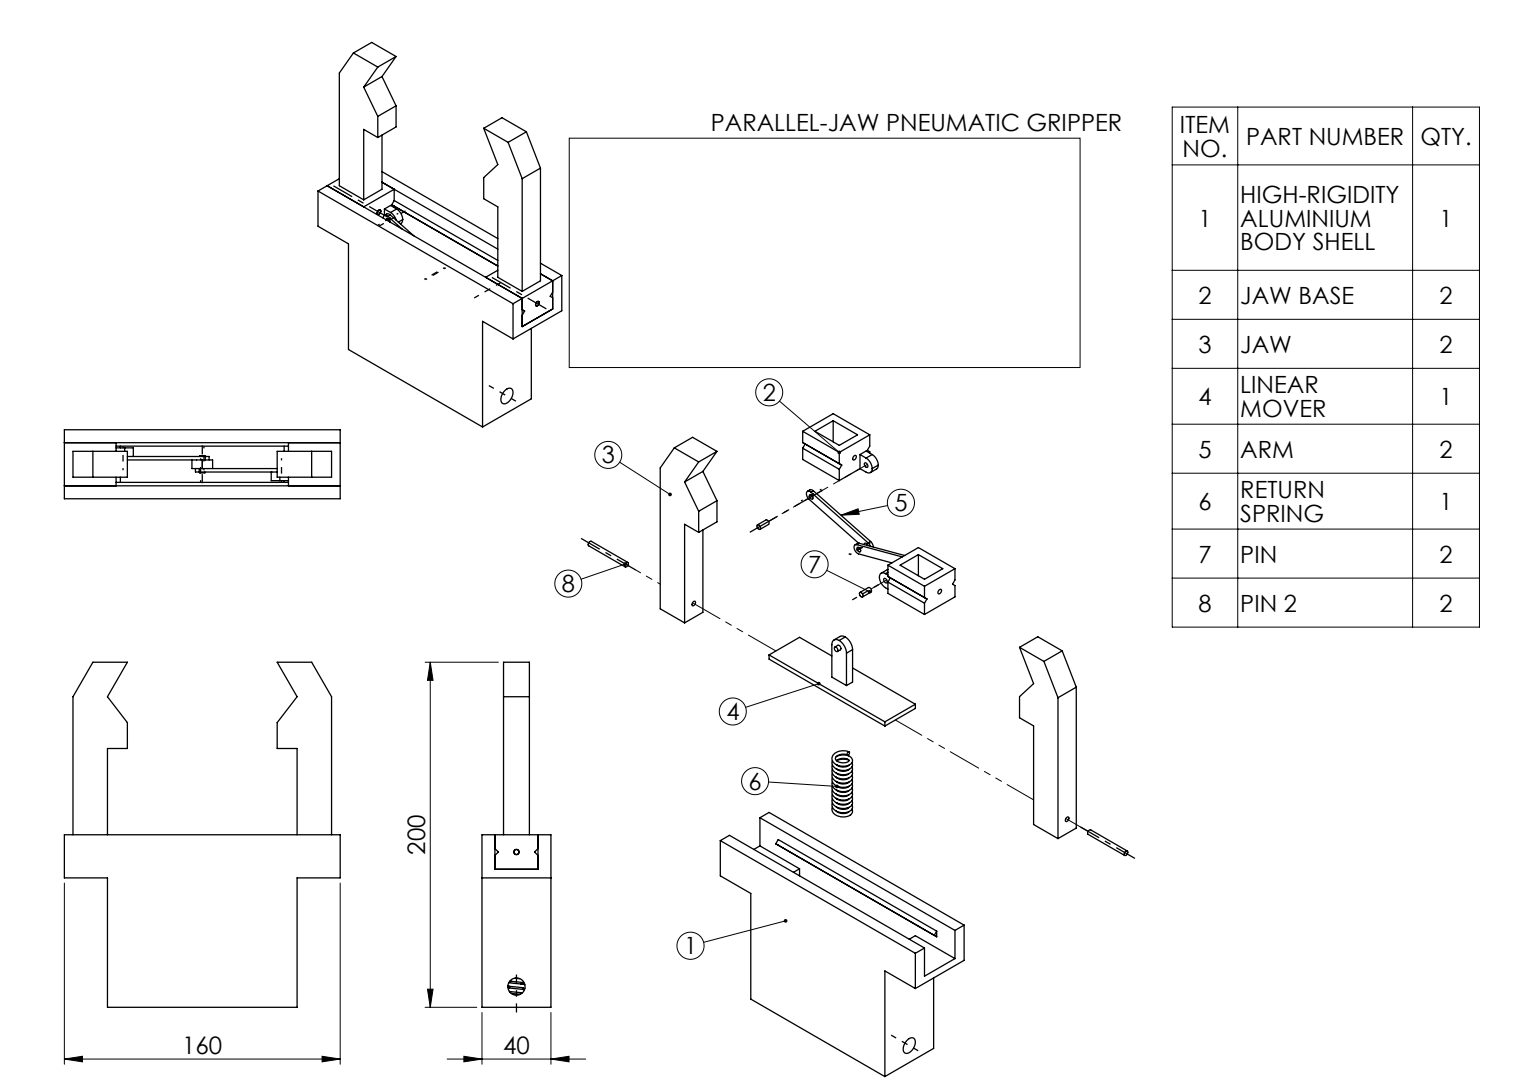
ISO-10303-21;
HEADER;
FILE_DESCRIPTION (('STEP AP214'),
    '1' );
FILE_NAME ('BR-001',
    '2026-10-04T07:56:41',
    ( '' ),
    ( '' ),
    'SwSTEP 2.0',
    'SolidWorks 2026',
    '' );
FILE_SCHEMA (( 'AUTOMOTIVE_DESIGN' ));
ENDSEC;

DATA;
#1 = CARTESIAN_POINT ( 'NONE',  ( 2.179377348189627916, -63.64547149457072805, 7.030887037049939003 ) ) ;
#2 = DIRECTION ( 'NONE',  ( -0.000000000000000000, 2.775557561562891351E-16, -1.000000000000000000 ) ) ;
#3 = CARTESIAN_POINT ( 'NONE',  ( 1.529537955723794918, -69.64547149457074227, 5.030887037049945221 ) ) ;
#4 = CARTESIAN_POINT ( 'NONE',  ( -0.09506052544073731458, -60.49547149457074369, 4.999999999999997335 ) ) ;
#5 = LINE ( 'NONE', #7090, #369 ) ;
#6 = DIRECTION ( 'NONE',  ( -1.000000000000000000, 0.000000000000000000, -0.000000000000000000 ) ) ;
#7 = CARTESIAN_POINT ( 'NONE',  ( -3.015831842038216859, -60.30452850542926058, -3.989209796945429432 ) ) ;
#8 = CARTESIAN_POINT ( 'NONE',  ( -7.360235569667856304, -89.74547149457073658, -0.09995255151716124498 ) ) ;
#9 = VERTEX_POINT ( 'NONE', #7435 ) ;
#10 = CARTESIAN_POINT ( 'NONE',  ( -1.719659006605372076, -75.15452850542925489, -4.969112962950016588 ) ) ;
#11 = DIRECTION ( 'NONE',  ( 0.000000000000000000, -1.000000000000000000, 0.000000000000000000 ) ) ;
#12 = EDGE_CURVE ( 'NONE', #8085, #480, #389, .T. ) ;
#13 = SHAPE_DEFINITION_REPRESENTATION ( #5408, #1019 ) ;
#14 = LINE ( 'NONE', #7738, #5692 ) ;
#15 = CARTESIAN_POINT ( 'NONE',  ( -4.312004677470992142, -84.04547149457074795, 3.009306630940933758 ) ) ;
#16 = CARTESIAN_POINT ( 'NONE',  ( 4.332187097882923332, -97.00000000000000000, -0.04074656551593417581 ) ) ;
#17 = CARTESIAN_POINT ( 'NONE',  ( -2.610703060766926598, -69.04547149457074795, 1.773238653441125745 ) ) ;
#18 = CARTESIAN_POINT ( 'NONE',  ( 6.628020296210641149, -74.40452850542925489, -2.253526892787612645 ) ) ;
#19 = LINE ( 'NONE', #2774, #674 ) ;
#20 = CARTESIAN_POINT ( 'NONE',  ( 4.725907263620373833, -82.09547149457074511, 1.635492904037598283 ) ) ;
#21 = CARTESIAN_POINT ( 'NONE',  ( -5.257311121191324155, -60.75452850542925631, 0.09995255151729526277 ) ) ;
#22 = CARTESIAN_POINT ( 'NONE',  ( -2.862020680886492308, -91.20452850542926626, 4.100960146804039752 ) ) ;
#23 = CARTESIAN_POINT ( 'NONE',  ( -0.09506052544086251999, -66.00452850542926342, -6.999999999999997335 ) ) ;
#24 = CARTESIAN_POINT ( 'NONE',  ( -2.823794231030039015, -86.59547149457075932, -1.017458915287723364 ) ) ;
#25 = VECTOR ( 'NONE', #598, 1000.000000000000000 ) ;
#26 = VERTEX_POINT ( 'NONE', #1027 ) ;
#27 = DIRECTION ( 'NONE',  ( -0.9954714945707483498, -0.09506052544079827971, 1.047588144072330487E-14 ) ) ;
#28 = DIRECTION ( 'NONE',  ( 0.000000000000000000, -1.000000000000000000, 0.000000000000000000 ) ) ;
#29 = CARTESIAN_POINT ( 'NONE',  ( 4.194503406049339134, -89.55452850542926058, -3.171033256558100089 ) ) ;
#30 = EDGE_LOOP ( 'NONE', ( #2065, #6214, #5997, #4915, #7865, #4258, #7605, #3266 ) ) ;
#31 = CARTESIAN_POINT ( 'NONE',  ( 1.529537955723690779, -80.85452850542925773, -5.030887037049978971 ) ) ;
#32 = CARTESIAN_POINT ( 'NONE',  ( 2.493201789345269148, -59.55452850542924637, -1.934965279058294518 ) ) ;
#33 = CARTESIAN_POINT ( 'NONE',  ( 0.000000000000000000, 0.000000000000000000, 0.000000000000000000 ) ) ;
#34 = CARTESIAN_POINT ( 'NONE',  ( -1.719659006605370744, -90.15452850542922647, -4.969112962950016588 ) ) ;
#35 = CARTESIAN_POINT ( 'NONE',  ( 4.037591185471445243, -92.70452850542926626, -5.718994135553947977 ) ) ;
#36 = CARTESIAN_POINT ( 'NONE',  ( -3.015831842038128485, -81.19547149457073942, 3.989209796945492048 ) ) ;
#37 = CARTESIAN_POINT ( 'NONE',  ( 2.823794231030039903, -71.40452850542924068, -1.017458915287783316 ) ) ;
#38 = DIRECTION ( 'NONE',  ( -0.000000000000000000, -0.000000000000000000, -1.000000000000000000 ) ) ;
#39 = CARTESIAN_POINT ( 'NONE',  ( -5.999999999999988454, -100.0010000000000048, -2.499999999999999112 ) ) ;
#40 = CARTESIAN_POINT ( 'NONE',  ( 2.823794231030042123, -89.40452850542926910, -1.017458915287783316 ) ) ;
#41 = CARTESIAN_POINT ( 'NONE',  ( 2.179377348189484476, -95.85452850542924352, -7.030887037049986077 ) ) ;
#42 = VECTOR ( 'NONE', #3900, 1000.000000000000000 ) ;
#43 = EDGE_CURVE ( 'NONE', #1966, #5555, #3595, .T. ) ;
#44 = LINE ( 'NONE', #810, #6447 ) ;
#45 = CARTESIAN_POINT ( 'NONE',  ( 1.719659006605391394, -79.65452850542925489, 4.969112962950016588 ) ) ;
#46 = CARTESIAN_POINT ( 'NONE',  ( 2.369498399071079842, -94.84547149457073090, -6.969112962950057444 ) ) ;
#47 = FACE_OUTER_BOUND ( 'NONE', #854, .T. ) ;
#48 = DIRECTION ( 'NONE',  ( -0.000000000000000000, 1.000000000000000000, 2.775557561562891351E-16 ) ) ;
#49 = VECTOR ( 'NONE', #4022, 1000.000000000000000 ) ;
#50 = AXIS2_PLACEMENT_3D ( 'NONE', #6623, #6543, #5905 ) ;
#51 = CIRCLE ( 'NONE', #1949, 3.000000000000000000 ) ;
#52 = EDGE_CURVE ( 'NONE', #1530, #5461, #2216, .T. ) ;
#53 = CARTESIAN_POINT ( 'NONE',  ( -1.529537955723671905, -61.35452850542925773, 5.030887037049979860 ) ) ;
#54 = CARTESIAN_POINT ( 'NONE',  ( -4.191402346623057440, -87.19547149457073942, 5.607243785695398941 ) ) ;
#55 = VECTOR ( 'NONE', #6929, 1000.000000000000000 ) ;
#56 = ORIENTED_EDGE ( 'NONE', *, *, #5322, .F. ) ;
#57 = CARTESIAN_POINT ( 'NONE',  ( 5.257311121191341918, -71.25452850542923500, -0.09995255151729465215 ) ) ;
#58 = LINE ( 'NONE', #6301, #4909 ) ;
#59 = ITEM_DEFINED_TRANSFORMATION ( 'NONE', 'NONE', #6452,  #2840 ) ;
#60 = CARTESIAN_POINT ( 'NONE',  ( -1.500000000000001110, -27.00000000000000000, 5.000000000000000000 ) ) ;
#61 = CARTESIAN_POINT ( 'NONE',  ( 1.719659006605285922, -76.84547149457073090, -4.969112962950050338 ) ) ;
#62 = CARTESIAN_POINT ( 'NONE',  ( 4.269446988268172483, -97.00000000000001421, -0.4101805542161022777 ) ) ;
#63 = CARTESIAN_POINT ( 'NONE',  ( 0.8796985632579598091, -60.64547149457074227, 3.030887037049952326 ) ) ;
#64 = CARTESIAN_POINT ( 'NONE',  ( 5.895805022753404678, -68.55452850542926058, -4.407101234057908989 ) ) ;
#65 = CARTESIAN_POINT ( 'NONE',  ( -5.999999999999993783, -51.00000000000000711, -2.499999999999999112 ) ) ;
#66 = CARTESIAN_POINT ( 'NONE',  ( -4.194503406049384431, -77.44547149457075363, -3.171033256558012159 ) ) ;
#67 = CARTESIAN_POINT ( 'NONE',  ( 5.257311121191341918, -59.25452850542924210, -0.09995255151729465215 ) ) ;
#68 = CARTESIAN_POINT ( 'NONE',  ( -4.725907263620319654, -87.90452850542926910, 1.635492904037698647 ) ) ;
#69 = CARTESIAN_POINT ( 'NONE',  ( -4.191402346623179120, -72.30452850542926058, -5.607243785695311900 ) ) ;
#70 = EDGE_CURVE ( 'NONE', #8240, #6658, #3048, .T. ) ;
#71 = CARTESIAN_POINT ( 'NONE',  ( -2.823794231030039903, -77.59547149457073090, -1.017458915287723364 ) ) ;
#72 = VERTEX_POINT ( 'NONE', #594 ) ;
#73 = CARTESIAN_POINT ( 'NONE',  ( 3.943604702053941724E-15, -27.99999999999999645, 0.000000000000000000 ) ) ;
#74 = CARTESIAN_POINT ( 'NONE',  ( 54.99999999999999289, 1.301042606982605715E-15, -7.500000000000002665 ) ) ;
#75 = CARTESIAN_POINT ( 'NONE',  ( 2.862020680886515400, -86.70452850542925205, -4.100960146804039752 ) ) ;
#76 = EDGE_LOOP ( 'NONE', ( #356, #276, #5543, #6009 ) ) ;
#77 = CARTESIAN_POINT ( 'NONE',  ( -1.529537955723670128, -79.35452850542925773, 5.030887037049979860 ) ) ;
#78 = CARTESIAN_POINT ( 'NONE',  ( -2.610703060766966566, -63.45452850542924494, -1.773238653441072232 ) ) ;
#79 = DIRECTION ( 'NONE',  ( -1.000000000000000000, 0.000000000000000000, 0.000000000000000000 ) ) ;
#80 = CARTESIAN_POINT ( 'NONE',  ( -2.862020680886493640, -82.20452850542925205, 4.100960146804039752 ) ) ;
#81 = CARTESIAN_POINT ( 'NONE',  ( 2.369498399071075845, -64.84547149457071669, -6.969112962950057444 ) ) ;
#82 = CARTESIAN_POINT ( 'NONE',  ( 1.069819614139556396, -70.65452850542925489, 2.969112962950023249 ) ) ;
#83 = EDGE_CURVE ( 'NONE', #4707, #1590, #2672, .T. ) ;
#84 = DIRECTION ( 'NONE',  ( 0.000000000000000000, -1.000000000000000000, -1.734723475976807094E-16 ) ) ;
#85 = DIRECTION ( 'NONE',  ( 0.000000000000000000, 0.000000000000000000, 1.000000000000000000 ) ) ;
#86 = CARTESIAN_POINT ( 'NONE',  ( 3.154386672714810658, -89.25452850542926342, -0.09995255151727241993 ) ) ;
#87 = CARTESIAN_POINT ( 'NONE',  ( 4.191402346623199549, -94.80452850542926058, 5.607243785695311900 ) ) ;
#88 = FACE_OUTER_BOUND ( 'NONE', #2763, .T. ) ;
#89 = CARTESIAN_POINT ( 'NONE',  ( 1.529537955723689890, -74.85452850542925773, -5.030887037049978971 ) ) ;
#90 = CARTESIAN_POINT ( 'NONE',  ( -5.895805022753476621, -89.44547149457073942, -4.407101234057782868 ) ) ;
#91 = DIRECTION ( 'NONE',  ( 1.000000000000000000, -0.000000000000000000, -0.000000000000000000 ) ) ;
#92 = CARTESIAN_POINT ( 'NONE',  ( -47.50000000000000711, 47.23441352194253540, 12.50000000000001954 ) ) ;
#93 = CARTESIAN_POINT ( 'NONE',  ( -0.09506052544075821453, -63.49547149457075079, 2.999999999999997780 ) ) ;
#94 = ADVANCED_FACE ( 'NONE', ( #2381 ), #5021, .T. ) ;
#95 = CARTESIAN_POINT ( 'NONE',  ( -4.312004677471060532, -60.45452850542923784, -3.009306630940844052 ) ) ;
#96 = CARTESIAN_POINT ( 'NONE',  ( -6.013306294175058575, -87.04547149457074795, 4.245374608440741326 ) ) ;
#97 = VERTEX_POINT ( 'NONE', #4421 ) ;
#98 = AXIS2_PLACEMENT_3D ( 'NONE', #2797, #1653, #1018 ) ;
#99 = CARTESIAN_POINT ( 'NONE',  ( -3.015831842038215083, -75.30452850542926058, -3.989209796945429432 ) ) ;
#100 = CARTESIAN_POINT ( 'NONE',  ( 50.00000000000000000, -1.734723475976807094E-15, 12.50000000000000000 ) ) ;
#101 = CARTESIAN_POINT ( 'NONE',  ( 46.73922289128223895, -17.64104216824340199, 4.500000000000000888 ) ) ;
#102 = EDGE_CURVE ( 'NONE', #5844, #6402, #2825, .T. ) ;
#103 = CARTESIAN_POINT ( 'NONE',  ( 2.862020680886599333, -78.79547149457074795, 4.100960146803977580 ) ) ;
#104 = DIRECTION ( 'NONE',  ( 0.000000000000000000, -1.000000000000000000, 0.000000000000000000 ) ) ;
#105 = CARTESIAN_POINT ( 'NONE',  ( -1.840261337453202639, -60.19547149457074653, 2.371175808195584267 ) ) ;
#106 = CARTESIAN_POINT ( 'NONE',  ( 6.686770931921523164, -65.10452850542924352, 2.072711028461649008 ) ) ;
#107 = LINE ( 'NONE', #2692, #5969 ) ;
#108 = CARTESIAN_POINT ( 'NONE',  ( 1.529537955723795584, -81.64547149457074227, 5.030887037049945221 ) ) ;
#109 = DIRECTION ( 'NONE',  ( -0.000000000000000000, 0.000000000000000000, -1.000000000000000000 ) ) ;
#110 = CARTESIAN_POINT ( 'NONE',  ( 3.015831842038235511, -88.80452850542926058, 3.989209796945429432 ) ) ;
#111 = CARTESIAN_POINT ( 'NONE',  ( -6.013306294175152722, -72.45452850542925205, -4.245374608440613429 ) ) ;
#112 = CARTESIAN_POINT ( 'NONE',  ( 3.154386672714809770, -79.24547149457073658, 0.09995255151720662534 ) ) ;
#113 = EDGE_CURVE ( 'NONE', #4681, #4928, #8269, .T. ) ;
#114 = ORIENTED_EDGE ( 'NONE', *, *, #1617, .T. ) ;
#115 = AXIS2_PLACEMENT_3D ( 'NONE', #3789, #4326, #6319 ) ;
#116 = DIRECTION ( 'NONE',  ( 0.000000000000000000, 0.000000000000000000, 1.000000000000000000 ) ) ;
#117 = CARTESIAN_POINT ( 'NONE',  ( 47.50000000000002132, 47.23441352194253540, 12.50000000000001954 ) ) ;
#118 = CARTESIAN_POINT ( 'NONE',  ( -2.862020680886492308, -91.20452850542926626, 4.100960146804039752 ) ) ;
#119 = ORIENTED_EDGE ( 'NONE', *, *, #70, .T. ) ;
#120 = CARTESIAN_POINT ( 'NONE',  ( 4.725907263620340970, -80.40452850542925489, -1.635492904037697981 ) ) ;
#121 = CARTESIAN_POINT ( 'NONE',  ( 2.610703060766946582, -88.54547149457074795, -1.773238653441125523 ) ) ;
#122 = DIRECTION ( 'NONE',  ( 1.000000000000000000, 0.000000000000000000, 0.000000000000000000 ) ) ;
#123 = CARTESIAN_POINT ( 'NONE',  ( -0.09506052544083921918, -84.00452850542926342, -4.999999999999997335 ) ) ;
#124 = AXIS2_PLACEMENT_3D ( 'NONE', #3381, #3919, #122 ) ;
#125 = CARTESIAN_POINT ( 'NONE',  ( 0.09506052544073236021, -61.99547149457073658, -6.999999999999997335 ) ) ;
#126 = VECTOR ( 'NONE', #38, 1000.000000000000000 ) ;
#127 = CARTESIAN_POINT ( 'NONE',  ( -1.840261337453252821, -69.30452850542926058, -2.371175808195547852 ) ) ;
#128 = FACE_OUTER_BOUND ( 'NONE', #7423, .T. ) ;
#129 = AXIS2_PLACEMENT_3D ( 'NONE', #1955, #4587, #1439 ) ;
#130 = DIRECTION ( 'NONE',  ( -1.000000000000000000, 0.000000000000000000, 0.000000000000000000 ) ) ;
#131 = CARTESIAN_POINT ( 'NONE',  ( 1.069819614139557284, -79.65452850542925489, 2.969112962950023249 ) ) ;
#132 = CARTESIAN_POINT ( 'NONE',  ( 7.360235569667880284, -92.25452850542926342, -0.09995255151731691212 ) ) ;
#133 = FACE_OUTER_BOUND ( 'NONE', #6862, .T. ) ;
#134 = CARTESIAN_POINT ( 'NONE',  ( -6.628020296210666018, -86.59547149457075932, -2.253526892787471869 ) ) ;
#135 = CARTESIAN_POINT ( 'NONE',  ( -65.00000000000000000, -7.999999999999992895, -12.50000000000000178 ) ) ;
#136 = CARTESIAN_POINT ( 'NONE',  ( -65.00000000000000000, -12.00000000000000711, 12.49999999999999822 ) ) ;
#137 = PRESENTATION_LAYER_ASSIGNMENT (  '', '', ( #6998 ) ) ;
#138 = CARTESIAN_POINT ( 'NONE',  ( -0.8796985632579439329, -68.14547149457074227, -3.030887037049952326 ) ) ;
#139 = CARTESIAN_POINT ( 'NONE',  ( -4.194503406049321370, -58.05452850542925347, 3.171033256558100533 ) ) ;
#140 = VERTEX_POINT ( 'NONE', #4384 ) ;
#141 = CARTESIAN_POINT ( 'NONE',  ( 4.312004677471075631, -73.95452850542926626, 3.009306630940844496 ) ) ;
#142 = CARTESIAN_POINT ( 'NONE',  ( -0.09506052544071266763, -87.49547149457075079, 6.999999999999997335 ) ) ;
#143 = ORIENTED_EDGE ( 'NONE', *, *, #1238, .T. ) ;
#144 = CARTESIAN_POINT ( 'NONE',  ( 0.09506052544086046607, -79.50452850542926342, 4.999999999999997335 ) ) ;
#145 = CARTESIAN_POINT ( 'NONE',  ( -80.00000000000000000, -50.00000000000000711, -12.50000000000000888 ) ) ;
#146 = CARTESIAN_POINT ( 'NONE',  ( 55.00000000000002132, -93.00000000000000000, 6.123233995736772199E-16 ) ) ;
#147 = CARTESIAN_POINT ( 'NONE',  ( -4.312004677470993030, -78.04547149457076216, 3.009306630940933758 ) ) ;
#148 = LINE ( 'NONE', #5288, #6329 ) ;
#149 = CARTESIAN_POINT ( 'NONE',  ( -2.610703060766927930, -63.04547149457074084, 1.773238653441125745 ) ) ;
#150 = CARTESIAN_POINT ( 'NONE',  ( -5.895805022753386915, -67.05452850542926058, 4.407101234057909878 ) ) ;
#151 = LINE ( 'NONE', #65, #1132 ) ;
#152 = CARTESIAN_POINT ( 'NONE',  ( -5.257311121191324155, -74.74547149457075079, -0.09995255151718371311 ) ) ;
#153 = SHAPE_REPRESENTATION ( 'pin 2', ( #2840 ), #1883 ) ;
#154 = LINE ( 'NONE', #7878, #4231 ) ;
#155 = CARTESIAN_POINT ( 'NONE',  ( 0.09506052544086084077, -82.50452850542926342, 4.999999999999997335 ) ) ;
#156 = CARTESIAN_POINT ( 'NONE',  ( 6.686770931921523164, -68.10452850542924352, 2.072711028461649008 ) ) ;
#157 = CARTESIAN_POINT ( 'NONE',  ( 0.8796985632579618075, -75.64547149457072805, 3.030887037049952326 ) ) ;
#158 = EDGE_CURVE ( 'NONE', #4876, #5889, #5061, .T. ) ;
#159 = EDGE_LOOP ( 'NONE', ( #4079, #1702, #1986 ) ) ;
#160 = FACE_OUTER_BOUND ( 'NONE', #6946, .T. ) ;
#161 = CARTESIAN_POINT ( 'NONE',  ( 2.862020680886516732, -95.70452850542926626, -4.100960146804039752 ) ) ;
#162 = CARTESIAN_POINT ( 'NONE',  ( 3.015831842038235511, -88.80452850542926058, 3.989209796945429432 ) ) ;
#163 = EDGE_LOOP ( 'NONE', ( #6818, #3032, #7905, #4249 ) ) ;
#164 = CARTESIAN_POINT ( 'NONE',  ( -2.862020680886494084, -79.20452850542925205, 4.100960146804039752 ) ) ;
#165 = CARTESIAN_POINT ( 'NONE',  ( -3.154386672714787565, -89.74547149457073658, -0.09995255151720625064 ) ) ;
#166 = CARTESIAN_POINT ( 'NONE',  ( 1.719659006605392504, -88.65452850542925489, 4.969112962950016588 ) ) ;
#167 = EDGE_CURVE ( 'NONE', #2862, #1798, #3763, .T. ) ;
#168 = CARTESIAN_POINT ( 'NONE',  ( -6.013306294175062128, -60.04547149457073374, 4.245374608440741326 ) ) ;
#169 = CARTESIAN_POINT ( 'NONE',  ( -1.686450176301567350, -64.20452850542925205, 2.482926158054133303 ) ) ;
#170 = CARTESIAN_POINT ( 'NONE',  ( 80.00000000000000000, 0.000000000000000000, 20.00000000000000000 ) ) ;
#171 = FACE_OUTER_BOUND ( 'NONE', #565, .T. ) ;
#172 = CARTESIAN_POINT ( 'NONE',  ( 0.8796985632578988579, -74.85452850542925773, -3.030887037049972310 ) ) ;
#173 = CARTESIAN_POINT ( 'NONE',  ( -2.179377348189460051, -88.35452850542924352, 7.030887037049988741 ) ) ;
#174 = CARTESIAN_POINT ( 'NONE',  ( 1.500000000000002442, -27.00000000000000000, 5.000000000000000000 ) ) ;
#175 = CARTESIAN_POINT ( 'NONE',  ( -4.037591185471542943, -89.29547149457074795, -5.718994135553860936 ) ) ;
#176 = CYLINDRICAL_SURFACE ( 'NONE', #6965, 5.000000000000004441 ) ;
#177 = LINE ( 'NONE', #1487, #3670 ) ;
#178 = CARTESIAN_POINT ( 'NONE',  ( -1.069819614139475794, -66.34547149457073090, 2.969112962950044121 ) ) ;
#179 = CARTESIAN_POINT ( 'NONE',  ( -4.725907263620323207, -63.90452850542925489, 1.635492904037698647 ) ) ;
#180 = VECTOR ( 'NONE', #3060, 1000.000000000000000 ) ;
#181 = ORIENTED_EDGE ( 'NONE', *, *, #5142, .F. ) ;
#182 = CARTESIAN_POINT ( 'NONE',  ( 5.257311121191341918, -71.25452850542923500, -0.09995255151729465215 ) ) ;
#183 = CARTESIAN_POINT ( 'NONE',  ( 0.09506052544073499699, -82.99547149457075079, -6.999999999999997335 ) ) ;
#184 = VERTEX_POINT ( 'NONE', #4941 ) ;
#185 = CARTESIAN_POINT ( 'NONE',  ( 1.529537955723690112, -77.85452850542922931, -5.030887037049978971 ) ) ;
#186 = EDGE_CURVE ( 'NONE', #2522, #3855, #7004, .T. ) ;
#187 = VECTOR ( 'NONE', #1383, 1000.000000000000000 ) ;
#188 = PLANE ( 'NONE',  #457 ) ;
#189 = AXIS2_PLACEMENT_3D ( 'NONE', #3637, #5920, #5243 ) ;
#190 = VECTOR ( 'NONE', #1369, 1000.000000000000000 ) ;
#191 = CARTESIAN_POINT ( 'NONE',  ( 3.015831842038148025, -70.69547149457073942, -3.989209796945492048 ) ) ;
#192 = FACE_OUTER_BOUND ( 'NONE', #662, .T. ) ;
#193 = CARTESIAN_POINT ( 'NONE',  ( -1.686450176301618642, -65.29547149457073374, -2.482926158054096000 ) ) ;
#194 = CARTESIAN_POINT ( 'NONE',  ( 7.360235569667877620, -74.25452850542924921, -0.09995255151731691212 ) ) ;
#195 = CARTESIAN_POINT ( 'NONE',  ( 80.00000000000000000, 0.000000000000000000, 20.00000000000000000 ) ) ;
#196 = FILL_AREA_STYLE_COLOUR ( '', #1408 ) ;
#197 = CARTESIAN_POINT ( 'NONE',  ( 1.529537955723691001, -83.85452850542927195, -5.030887037049978971 ) ) ;
#198 = CARTESIAN_POINT ( 'NONE',  ( -6.628020296210623385, -63.90452850542925489, 2.253526892787613978 ) ) ;
#199 = CARTESIAN_POINT ( 'NONE',  ( -1.069819614139474906, -75.34547149457073090, 2.969112962950044121 ) ) ;
#200 = VERTEX_POINT ( 'NONE', #6335 ) ;
#201 = CARTESIAN_POINT ( 'NONE',  ( 80.00000000000000000, 0.000000000000000000, 20.00000000000000000 ) ) ;
#202 = CARTESIAN_POINT ( 'NONE',  ( -1.719659006605370744, -93.15452850542925489, -4.969112962950016588 ) ) ;
#203 = CARTESIAN_POINT ( 'NONE',  ( 4.725907263620340970, -83.40452850542925489, -1.635492904037697981 ) ) ;
#204 = VERTEX_POINT ( 'NONE', #1706 ) ;
#205 = CARTESIAN_POINT ( 'NONE',  ( 5.257311121191341030, -71.25452850542924921, -0.09995255151729466603 ) ) ;
#206 = CARTESIAN_POINT ( 'NONE',  ( 2.610703060766947914, -94.54547149457073374, -1.773238653441125523 ) ) ;
#207 = CARTESIAN_POINT ( 'NONE',  ( -4.194503406049315153, -91.05452850542923215, 3.171033256558100533 ) ) ;
#208 = CARTESIAN_POINT ( 'NONE',  ( 6.013306294175077227, -61.54547149457074084, -4.245374608440741326 ) ) ;
#209 = CARTESIAN_POINT ( 'NONE',  ( -1.840261337453252821, -66.30452850542926058, -2.371175808195547852 ) ) ;
#210 = VERTEX_POINT ( 'NONE', #510 ) ;
#211 = DIRECTION ( 'NONE',  ( 9.251858538542971581E-17, -1.000000000000000000, 0.000000000000000000 ) ) ;
#212 = CARTESIAN_POINT ( 'NONE',  ( -0.9662349396012467340, -27.25766265056033433, 4.500000000000000888 ) ) ;
#213 = CARTESIAN_POINT ( 'NONE',  ( -1.686450176301564907, -82.20452850542925205, 2.482926158054133303 ) ) ;
#214 = CARTESIAN_POINT ( 'NONE',  ( 2.179377348189483143, -86.85452850542924352, -7.030887037049986077 ) ) ;
#215 = CARTESIAN_POINT ( 'NONE',  ( -4.191402346623057440, -87.19547149457073942, 5.607243785695398941 ) ) ;
#216 = CARTESIAN_POINT ( 'NONE',  ( -5.999999999999992895, -50.00000000000000000, -2.499999999999999112 ) ) ;
#217 = DIRECTION ( 'NONE',  ( 0.000000000000000000, 0.7071067811865507924, -0.7071067811865441310 ) ) ;
#218 = CARTESIAN_POINT ( 'NONE',  ( -0.09506052544075743738, -69.49547149457075079, 2.999999999999997780 ) ) ;
#219 = UNCERTAINTY_MEASURE_WITH_UNIT (LENGTH_MEASURE( 1.000000000000000082E-05 ), #2470, 'distance_accuracy_value', 'NONE');
#220 = SURFACE_SIDE_STYLE ('',( #2333 ) ) ;
#221 = ORIENTED_EDGE ( 'NONE', *, *, #2206, .T. ) ;
#222 = ADVANCED_FACE ( 'NONE', ( #7515 ), #5686, .T. ) ;
#223 = CARTESIAN_POINT ( 'NONE',  ( -4.194503406049319594, -67.05452850542926058, 3.171033256558100533 ) ) ;
#224 = CARTESIAN_POINT ( 'NONE',  ( 6.628020296210687334, -79.09547149457075932, 2.253526892787472757 ) ) ;
#225 = SURFACE_STYLE_FILL_AREA ( #2174 ) ;
#226 = EDGE_CURVE ( 'NONE', #6118, #4574, #2581, .T. ) ;
#227 = ORIENTED_EDGE ( 'NONE', *, *, #6640, .F. ) ;
#228 = CARTESIAN_POINT ( 'NONE',  ( -5.257311121191324155, -63.75452850542925631, 0.09995255151729526277 ) ) ;
#229 = CARTESIAN_POINT ( 'NONE',  ( -5.999999999999993783, -51.00000000000000711, 2.500000000000000888 ) ) ;
#230 = CARTESIAN_POINT ( 'NONE',  ( -5.257311121191324155, -71.74547149457075079, -0.09995255151718371311 ) ) ;
#231 = CARTESIAN_POINT ( 'NONE',  ( -80.00100000000001899, -83.00000000000002842, 0.000000000000000000 ) ) ;
#232 = CARTESIAN_POINT ( 'NONE',  ( 1.719659006605287921, -97.84547149457071669, -4.969112962950050338 ) ) ;
#233 = CARTESIAN_POINT ( 'NONE',  ( 6.686770931921522276, -62.10452850542925063, 2.072711028461649008 ) ) ;
#234 = ORIENTED_EDGE ( 'NONE', *, *, #7378, .T. ) ;
#235 = CARTESIAN_POINT ( 'NONE',  ( 1.719659006605391616, -82.65452850542925489, 4.969112962950016588 ) ) ;
#236 = CARTESIAN_POINT ( 'NONE',  ( 6.628020296210639373, -62.40452850542925489, -2.253526892787612645 ) ) ;
#237 = CARTESIAN_POINT ( 'NONE',  ( 2.882544866740877065, -73.39547149457074227, -0.8366430509619593447 ) ) ;
#238 = VERTEX_POINT ( 'NONE', #7087 ) ;
#239 = DIRECTION ( 'NONE',  ( 0.000000000000000000, -0.000000000000000000, -1.000000000000000000 ) ) ;
#240 = CARTESIAN_POINT ( 'NONE',  ( 3.015831842038236399, -94.80452850542924637, 3.989209796945429432 ) ) ;
#241 = CARTESIAN_POINT ( 'NONE',  ( 1.529537955723690112, -77.85452850542922931, -5.030887037049978971 ) ) ;
#242 = ORIENTED_EDGE ( 'NONE', *, *, #358, .F. ) ;
#243 = CARTESIAN_POINT ( 'NONE',  ( -4.312004677471057867, -72.45452850542923784, -3.009306630940843608 ) ) ;
#244 = CARTESIAN_POINT ( 'NONE',  ( -0.8796985632579418235, -86.14547149457072805, -3.030887037049952326 ) ) ;
#245 = CARTESIAN_POINT ( 'NONE',  ( 2.862020680886601998, -96.79547149457073374, 4.100960146803977580 ) ) ;
#246 = CARTESIAN_POINT ( 'NONE',  ( 0.09506052544086046607, -79.50452850542926342, 4.999999999999997335 ) ) ;
#247 = CARTESIAN_POINT ( 'NONE',  ( 2.369498399071225947, -85.65452850542926910, 6.969112962950009482 ) ) ;
#248 = ADVANCED_FACE ( 'NONE', ( #3343 ), #5902, .T. ) ;
#249 = CARTESIAN_POINT ( 'NONE',  ( 1.686450176301584225, -68.70452850542925205, -2.482926158054133303 ) ) ;
#250 = VERTEX_POINT ( 'NONE', #3258 ) ;
#251 = FACE_OUTER_BOUND ( 'NONE', #7883, .T. ) ;
#252 = LINE ( 'NONE', #8058, #5108 ) ;
#253 = CARTESIAN_POINT ( 'NONE',  ( 1.686450176301585335, -77.70452850542925205, -2.482926158054133303 ) ) ;
#254 = CARTESIAN_POINT ( 'NONE',  ( 7.360235569667880284, -86.25452850542924921, -0.09995255151731691212 ) ) ;
#255 = AXIS2_PLACEMENT_3D ( 'NONE', #6696, #2244, #926 ) ;
#256 = CARTESIAN_POINT ( 'NONE',  ( 4.191402346623080533, -88.69547149457073942, -5.607243785695398941 ) ) ;
#257 = DIRECTION ( 'NONE',  ( 0.000000000000000000, 0.000000000000000000, 1.000000000000000000 ) ) ;
#258 = PRODUCT_RELATED_PRODUCT_CATEGORY ( 'part', '', ( #6217 ) ) ;
#259 = DIRECTION ( 'NONE',  ( 0.000000000000000000, 0.7071067811865442421, -0.7071067811865509034 ) ) ;
#260 = CARTESIAN_POINT ( 'NONE',  ( 0.09506052544077478461, -64.99547149457075079, -2.999999999999997780 ) ) ;
#261 = CARTESIAN_POINT ( 'NONE',  ( 46.73922289128223895, -17.64104216824340199, 4.500000000000000888 ) ) ;
#262 = ORIENTED_EDGE ( 'NONE', *, *, #5429, .F. ) ;
#263 = CARTESIAN_POINT ( 'NONE',  ( 3.015831842038232402, -64.80452850542926058, 3.989209796945429432 ) ) ;
#264 = CARTESIAN_POINT ( 'NONE',  ( 2.369498399071077177, -76.84547149457073090, -6.969112962950057444 ) ) ;
#265 = FILL_AREA_STYLE ('',( #2132 ) ) ;
#266 = CARTESIAN_POINT ( 'NONE',  ( 54.99999999999999289, -1.301042606982604729E-15, 7.499999999999997335 ) ) ;
#267 = VECTOR ( 'NONE', #2809, 1000.000000000000000 ) ;
#268 = CARTESIAN_POINT ( 'NONE',  ( -1.719659006605265716, -75.34547149457074511, 4.969112962950051227 ) ) ;
#269 = CARTESIAN_POINT ( 'NONE',  ( -0.09506052544084110656, -69.00452850542926342, -4.999999999999997335 ) ) ;
#270 = DIRECTION ( 'NONE',  ( -0.000000000000000000, -0.000000000000000000, -1.000000000000000000 ) ) ;
#271 = CIRCLE ( 'NONE', #522, 5.000000000000000888 ) ;
#272 = CARTESIAN_POINT ( 'NONE',  ( -4.784657899331159925, -65.89547149457074227, 1.454677039711874675 ) ) ;
#273 = DIRECTION ( 'NONE',  ( 0.000000000000000000, 0.000000000000000000, 1.000000000000000000 ) ) ;
#274 = CARTESIAN_POINT ( 'NONE',  ( -4.784657899331155484, -95.89547149457074227, 1.454677039711874675 ) ) ;
#275 = CARTESIAN_POINT ( 'NONE',  ( -6.013306294175153610, -60.45452850542925916, -4.245374608440613429 ) ) ;
#276 = ORIENTED_EDGE ( 'NONE', *, *, #1868, .F. ) ;
#277 = ADVANCED_FACE ( 'NONE', ( #133 ), #3970, .F. ) ;
#278 = FILL_AREA_STYLE ('',( #196 ) ) ;
#279 = CARTESIAN_POINT ( 'NONE',  ( 1.529537955723690557, -80.85452850542925773, -5.030887037049978971 ) ) ;
#280 = EDGE_CURVE ( 'NONE', #6915, #2088, #1958, .T. ) ;
#281 = ORIENTED_EDGE ( 'NONE', *, *, #3692, .F. ) ;
#282 = DIRECTION ( 'NONE',  ( 0.000000000000000000, -2.775557561562891351E-16, 1.000000000000000000 ) ) ;
#283 = CARTESIAN_POINT ( 'NONE',  ( -4.312004677471056091, -87.45452850542925205, -3.009306630940844052 ) ) ;
#284 = CARTESIAN_POINT ( 'NONE',  ( -1.529537955723669684, -82.35452850542922931, 5.030887037049979860 ) ) ;
#285 = ORIENTED_EDGE ( 'NONE', *, *, #8144, .T. ) ;
#286 = CARTESIAN_POINT ( 'NONE',  ( -0.09506052544084110656, -69.00452850542926342, -4.999999999999997335 ) ) ;
#287 = CARTESIAN_POINT ( 'NONE',  ( 2.493201789345311337, -87.94547149457073942, 1.934965279058241006 ) ) ;
#288 = CARTESIAN_POINT ( 'NONE',  ( -2.493201789345293129, -59.44547149457074653, -1.934965279058240561 ) ) ;
#289 = CARTESIAN_POINT ( 'NONE',  ( 1.719659006605391172, -76.65452850542922647, 4.969112962950016588 ) ) ;
#290 = CARTESIAN_POINT ( 'NONE',  ( 6.628020296210642037, -86.40452850542926910, -2.253526892787612645 ) ) ;
#291 = ADVANCED_FACE ( 'NONE', ( #7854, #719 ), #1914, .F. ) ;
#292 = CARTESIAN_POINT ( 'NONE',  ( -2.493201789345288688, -95.44547149457075363, -1.934965279058240561 ) ) ;
#293 = VERTEX_POINT ( 'NONE', #7045 ) ;
#294 = CARTESIAN_POINT ( 'NONE',  ( 6.123233995736760366E-16, -27.00000000000000000, -5.000000000000000000 ) ) ;
#295 = CARTESIAN_POINT ( 'NONE',  ( 54.99999999999999289, 1.301042606982605715E-15, -7.500000000000002665 ) ) ;
#296 = CARTESIAN_POINT ( 'NONE',  ( 1.840261337453271473, -82.80452850542926058, 2.371175808195547852 ) ) ;
#297 = CARTESIAN_POINT ( 'NONE',  ( -7.360235569667856304, -87.75452850542924921, 0.09995255151731782806 ) ) ;
#298 = CARTESIAN_POINT ( 'NONE',  ( 2.369498399071078065, -79.84547149457074511, -6.969112962950057444 ) ) ;
#299 = CARTESIAN_POINT ( 'NONE',  ( 50.00000000000000000, 1.734723475976807094E-15, -12.50000000000000000 ) ) ;
#300 = CARTESIAN_POINT ( 'NONE',  ( 2.862020680886601554, -93.79547149457074795, 4.100960146803977580 ) ) ;
#301 = CARTESIAN_POINT ( 'NONE',  ( -0.8796985632578785408, -82.35452850542927195, 3.030887037049973198 ) ) ;
#302 = UNCERTAINTY_MEASURE_WITH_UNIT (LENGTH_MEASURE( 1.000000000000000082E-05 ), #4684, 'distance_accuracy_value', 'NONE');
#303 = FACE_OUTER_BOUND ( 'NONE', #1052, .T. ) ;
#304 = ORIENTED_EDGE ( 'NONE', *, *, #4864, .F. ) ;
#305 = CARTESIAN_POINT ( 'NONE',  ( 54.99999999999999289, -9.999999999999994671, -1.500000000000000666 ) ) ;
#306 = CARTESIAN_POINT ( 'NONE',  ( -5.257311121191324155, -63.75452850542925631, 0.09995255151729526277 ) ) ;
#307 = CARTESIAN_POINT ( 'NONE',  ( -2.369498399071056305, -84.34547149457075932, 6.969112962950058332 ) ) ;
#308 = ORIENTED_EDGE ( 'NONE', *, *, #7858, .F. ) ;
#309 = CARTESIAN_POINT ( 'NONE',  ( 1.529537955723795584, -75.64547149457072805, 5.030887037049945221 ) ) ;
#310 = CARTESIAN_POINT ( 'NONE',  ( 4.784657899331176800, -73.39547149457074227, -1.454677039711874009 ) ) ;
#311 = CARTESIAN_POINT ( 'NONE',  ( -4.194503406049319594, -67.05452850542926058, 3.171033256558100533 ) ) ;
#312 = CARTESIAN_POINT ( 'NONE',  ( -5.999999999999988454, -100.0010000000000048, 2.500000000000000888 ) ) ;
#313 = CARTESIAN_POINT ( 'NONE',  ( 1.529537955723795140, -69.64547149457074227, 5.030887037049945221 ) ) ;
#314 = CARTESIAN_POINT ( 'NONE',  ( 45.00000000000000000, -14.99999999999999467, 4.499999999999999112 ) ) ;
#315 = CARTESIAN_POINT ( 'NONE',  ( -6.686770931921508954, -57.60452850542926484, -2.072711028461647675 ) ) ;
#316 = ORIENTED_EDGE ( 'NONE', *, *, #6930, .F. ) ;
#317 = AXIS2_PLACEMENT_3D ( 'NONE', #4788, #4662, #4742 ) ;
#318 = LINE ( 'NONE', #2975, #6253 ) ;
#319 = AXIS2_PLACEMENT_3D ( 'NONE', #8320, #7056, #3853 ) ;
#320 = ORIENTED_EDGE ( 'NONE', *, *, #4393, .F. ) ;
#321 = CARTESIAN_POINT ( 'NONE',  ( 55.00000000000000000, -25.00000000000002132, 20.00000000000000000 ) ) ;
#322 = CARTESIAN_POINT ( 'NONE',  ( -4.194503406049315153, -88.05452850542921794, 3.171033256558100533 ) ) ;
#323 = CARTESIAN_POINT ( 'NONE',  ( -4.312004677471057867, -78.45452850542925205, -3.009306630940844052 ) ) ;
#324 = ORIENTED_EDGE ( 'NONE', *, *, #6025, .F. ) ;
#325 = CARTESIAN_POINT ( 'NONE',  ( 1.719659006605389839, -67.65452850542925489, 4.969112962950015699 ) ) ;
#326 = CARTESIAN_POINT ( 'NONE',  ( 0.09506052544077665811, -79.99547149457075079, -2.999999999999997780 ) ) ;
#327 = CARTESIAN_POINT ( 'NONE',  ( -4.312004677470990366, -96.04547149457074795, 3.009306630940933758 ) ) ;
#328 = EDGE_CURVE ( 'NONE', #3916, #5740, #1998, .T. ) ;
#329 = CARTESIAN_POINT ( 'NONE',  ( -4.194503406049316929, -73.05452850542926058, 3.171033256558100533 ) ) ;
#330 = CARTESIAN_POINT ( 'NONE',  ( -6.013306294175149169, -87.45452850542925205, -4.245374608440613429 ) ) ;
#331 = CARTESIAN_POINT ( 'NONE',  ( 2.823794231030038571, -59.40452850542925489, -1.017458915287783316 ) ) ;
#332 = ORIENTED_EDGE ( 'NONE', *, *, #7144, .F. ) ;
#333 = PLANE ( 'NONE',  #3355 ) ;
#334 = ORIENTED_EDGE ( 'NONE', *, *, #1098, .F. ) ;
#335 = DIRECTION ( 'NONE',  ( 0.000000000000000000, -1.000000000000000000, 0.000000000000000000 ) ) ;
#336 = CARTESIAN_POINT ( 'NONE',  ( 2.823794231030039903, -71.40452850542924068, -1.017458915287783316 ) ) ;
#337 = CARTESIAN_POINT ( 'NONE',  ( -6.013306294175152722, -78.45452850542925205, -4.245374608440613429 ) ) ;
#338 = CARTESIAN_POINT ( 'NONE',  ( -6.628020296210667794, -80.59547149457075932, -2.253526892787471869 ) ) ;
#339 = CARTESIAN_POINT ( 'NONE',  ( 6.000000000000012434, -50.00000000000000000, 2.500000000000000888 ) ) ;
#340 = CARTESIAN_POINT ( 'NONE',  ( -4.784657899331155484, -95.89547149457074227, 1.454677039711874675 ) ) ;
#341 = CARTESIAN_POINT ( 'NONE',  ( 0.8796985632579006342, -89.85452850542924352, -3.030887037049972310 ) ) ;
#342 = SURFACE_STYLE_USAGE ( .BOTH. , #220 ) ;
#343 = ORIENTED_EDGE ( 'NONE', *, *, #113, .F. ) ;
#344 = CARTESIAN_POINT ( 'NONE',  ( 80.00000000000000000, -9.999999999999991118, -10.50000000000000888 ) ) ;
#345 = CARTESIAN_POINT ( 'NONE',  ( -2.882544866740875289, -93.60452850542925773, -0.8366430509618996147 ) ) ;
#346 = CARTESIAN_POINT ( 'NONE',  ( 5.895805022753496161, -84.94547149457073942, 4.407101234057782868 ) ) ;
#347 = AXIS2_PLACEMENT_3D ( 'NONE', #2756, #5316, #6516 ) ;
#348 = VERTEX_POINT ( 'NONE', #4548 ) ;
#349 = CARTESIAN_POINT ( 'NONE',  ( 4.194503406049401306, -72.94547149457073942, 3.171033256558012159 ) ) ;
#350 = CARTESIAN_POINT ( 'NONE',  ( -5.257311121191324155, -71.74547149457075079, -0.09995255151718371311 ) ) ;
#351 = CARTESIAN_POINT ( 'NONE',  ( -4.312004677471058756, -69.45452850542925205, -3.009306630940844052 ) ) ;
#352 = FACE_OUTER_BOUND ( 'NONE', #3772, .T. ) ;
#353 = EDGE_CURVE ( 'NONE', #6629, #3744, #7681, .T. ) ;
#354 = CARTESIAN_POINT ( 'NONE',  ( -4.725907263620354293, -68.59547149457073090, -1.635492904037597617 ) ) ;
#355 = CARTESIAN_POINT ( 'NONE',  ( 2.369498399071222838, -58.65452850542925489, 6.969112962950009482 ) ) ;
#356 = ORIENTED_EDGE ( 'NONE', *, *, #5085, .F. ) ;
#357 = LINE ( 'NONE', #7564, #55 ) ;
#358 = EDGE_CURVE ( 'NONE', #1800, #6097, #1314, .T. ) ;
#359 = EDGE_CURVE ( 'NONE', #1450, #210, #2081, .T. ) ;
#360 = ORIENTED_EDGE ( 'NONE', *, *, #1284, .T. ) ;
#361 = CYLINDRICAL_SURFACE ( 'NONE', #5299, 4.000000000000000000 ) ;
#362 = CARTESIAN_POINT ( 'NONE',  ( 5.257311121191341918, -83.25452850542926342, -0.09995255151729465215 ) ) ;
#363 = CARTESIAN_POINT ( 'NONE',  ( 4.725907263620340082, -74.40452850542925489, -1.635492904037697981 ) ) ;
#364 = CARTESIAN_POINT ( 'NONE',  ( -4.194503406049317817, -76.05452850542926058, 3.171033256558101865 ) ) ;
#365 = CARTESIAN_POINT ( 'NONE',  ( 2.610703060766946138, -79.54547149457074795, -1.773238653441125523 ) ) ;
#366 = CARTESIAN_POINT ( 'NONE',  ( 5.257311121191343695, -97.24547149457075079, 0.09995255151718437925 ) ) ;
#367 = CARTESIAN_POINT ( 'NONE',  ( -4.312004677471058756, -69.45452850542925205, -3.009306630940844052 ) ) ;
#368 = CARTESIAN_POINT ( 'NONE',  ( -4.191402346623178232, -84.30452850542926058, -5.607243785695311900 ) ) ;
#369 = VECTOR ( 'NONE', #5147, 1000.000000000000000 ) ;
#370 = CARTESIAN_POINT ( 'NONE',  ( 0.09506052544083654077, -58.50452850542925631, 2.999999999999997780 ) ) ;
#371 = PRODUCT_CONTEXT ( 'NONE', #2292, 'mechanical' ) ;
#372 = ORIENTED_EDGE ( 'NONE', *, *, #7078, .F. ) ;
#373 = CARTESIAN_POINT ( 'NONE',  ( 75.00000000000000000, -19.99999999999999645, -7.500000000000006217 ) ) ;
#374 = EDGE_CURVE ( 'NONE', #238, #5682, #7173, .T. ) ;
#375 = ORIENTED_EDGE ( 'NONE', *, *, #3835, .T. ) ;
#376 = FACE_OUTER_BOUND ( 'NONE', #2659, .T. ) ;
#377 = CARTESIAN_POINT ( 'NONE',  ( -0.09506052544081970701, -72.00452850542926342, -2.999999999999997780 ) ) ;
#378 = CARTESIAN_POINT ( 'NONE',  ( 6.013306294175077227, -79.54547149457074795, -4.245374608440741326 ) ) ;
#379 = LINE ( 'NONE', #7299, #1182 ) ;
#380 = LINE ( 'NONE', #4853, #7186 ) ;
#381 = CARTESIAN_POINT ( 'NONE',  ( -2.610703060766964345, -81.45452850542925205, -1.773238653441072232 ) ) ;
#382 = CARTESIAN_POINT ( 'NONE',  ( -55.00000000000000000, -25.00000000000002132, 20.00000000000000000 ) ) ;
#383 = EDGE_LOOP ( 'NONE', ( #4327, #3791, #8225, #2640 ) ) ;
#384 = DIRECTION ( 'NONE',  ( -1.000000000000000000, 0.000000000000000000, 0.000000000000000000 ) ) ;
#385 = CARTESIAN_POINT ( 'NONE',  ( 0.09506052544084107880, -94.50452850542926342, 2.999999999999997780 ) ) ;
#386 = AXIS2_PLACEMENT_3D ( 'NONE', #1428, #3953, #5087 ) ;
#387 = CARTESIAN_POINT ( 'NONE',  ( -7.360235569667858968, -68.74547149457075079, -0.09995255151716124498 ) ) ;
#388 =( NAMED_UNIT ( * ) PLANE_ANGLE_UNIT ( ) SI_UNIT ( $, .RADIAN. ) );
#389 = LINE ( 'NONE', #6796, #1413 ) ;
#390 = CARTESIAN_POINT ( 'NONE',  ( 4.194503406049403083, -75.94547149457073942, 3.171033256558012159 ) ) ;
#391 = CARTESIAN_POINT ( 'NONE',  ( -0.09506052544073655131, -66.49547149457075079, 4.999999999999997335 ) ) ;
#392 = CARTESIAN_POINT ( 'NONE',  ( 4.194503406049335581, -65.55452850542923215, -3.171033256558100089 ) ) ;
#393 = CARTESIAN_POINT ( 'NONE',  ( 43.45299461620743386, -9.999999999999994671, 0.000000000000000000 ) ) ;
#394 = AXIS2_PLACEMENT_3D ( 'NONE', #5609, #3678, #6487 ) ;
#395 = CIRCLE ( 'NONE', #1478, 1.499999999999999556 ) ;
#396 =( REPRESENTATION_RELATIONSHIP ('NONE','NONE', #4188, #1066 ) REPRESENTATION_RELATIONSHIP_WITH_TRANSFORMATION ( #6468 )SHAPE_REPRESENTATION_RELATIONSHIP( ) );
#397 = AXIS2_PLACEMENT_3D ( 'NONE', #4050, #2120, #1311 ) ;
#398 = CARTESIAN_POINT ( 'NONE',  ( 3.015831842038147137, -64.69547149457075363, -3.989209796945492048 ) ) ;
#399 = SURFACE_SIDE_STYLE ('',( #1115 ) ) ;
#400 = CARTESIAN_POINT ( 'NONE',  ( 4.312004677471079184, -94.95452850542926626, 3.009306630940844496 ) ) ;
#401 = ORIENTED_EDGE ( 'NONE', *, *, #6218, .F. ) ;
#402 = CARTESIAN_POINT ( 'NONE',  ( 0.7729879516809982087, -29.89870481880373987, 4.500000000000000888 ) ) ;
#403 = ORIENTED_EDGE ( 'NONE', *, *, #1284, .F. ) ;
#404 = CARTESIAN_POINT ( 'NONE',  ( 1.500000000000002442, -27.00000000000000000, -5.000000000000000000 ) ) ;
#405 = CARTESIAN_POINT ( 'NONE',  ( -2.862020680886492752, -88.20452850542925205, 4.100960146804039752 ) ) ;
#406 = CARTESIAN_POINT ( 'NONE',  ( -4.784657899331190123, -78.60452850542925773, -1.454677039711773867 ) ) ;
#407 = EDGE_CURVE ( 'NONE', #3855, #7622, #7218, .T. ) ;
#408 = CARTESIAN_POINT ( 'NONE',  ( -4.725907263620323207, -63.90452850542925489, 1.635492904037698647 ) ) ;
#409 = CARTESIAN_POINT ( 'NONE',  ( -2.823794231030039459, -83.59547149457075932, -1.017458915287723364 ) ) ;
#410 = CARTESIAN_POINT ( 'NONE',  ( -0.09506052544075858923, -60.49547149457073658, 2.999999999999997780 ) ) ;
#411 = CARTESIAN_POINT ( 'NONE',  ( 5.257311121191341918, -68.25452850542926342, -0.09995255151729465215 ) ) ;
#412 = CARTESIAN_POINT ( 'NONE',  ( 4.037591185471443467, -83.70452850542925205, -5.718994135553947977 ) ) ;
#413 = CARTESIAN_POINT ( 'NONE',  ( 2.610703060766947914, -97.54547149457074795, -1.773238653441125523 ) ) ;
#414 = EDGE_CURVE ( 'NONE', #7949, #1490, #44, .T. ) ;
#415 = ORIENTED_EDGE ( 'NONE', *, *, #5724, .T. ) ;
#416 = CARTESIAN_POINT ( 'NONE',  ( 80.00000000000000000, 0.000000000000000000, 20.00000000000000000 ) ) ;
#417 = VERTEX_POINT ( 'NONE', #8308 ) ;
#418 = CARTESIAN_POINT ( 'NONE',  ( -1.529537955723668574, -91.35452850542924352, 5.030887037049979860 ) ) ;
#419 = CARTESIAN_POINT ( 'NONE',  ( -0.09506052544082045641, -66.00452850542926342, -2.999999999999997780 ) ) ;
#420 = CARTESIAN_POINT ( 'NONE',  ( -5.895805022753477509, -80.44547149457073942, -4.407101234057782868 ) ) ;
#421 = DIRECTION ( 'NONE',  ( -1.261617073437677752E-16, 1.000000000000000000, 0.000000000000000000 ) ) ;
#422 = CARTESIAN_POINT ( 'NONE',  ( 0.09506052544075753452, -94.99547149457073658, -4.999999999999997335 ) ) ;
#423 = CARTESIAN_POINT ( 'NONE',  ( -2.882544866740876177, -84.60452850542927195, -0.8366430509618996147 ) ) ;
#424 = FACE_OUTER_BOUND ( 'NONE', #5365, .T. ) ;
#425 = VERTEX_POINT ( 'NONE', #5144 ) ;
#426 = CARTESIAN_POINT ( 'NONE',  ( 45.96623493960122886, -14.74233734943963192, 2.500000000000000888 ) ) ;
#427 = CARTESIAN_POINT ( 'NONE',  ( -5.257311121191324155, -60.75452850542925631, 0.09995255151729526277 ) ) ;
#428 = CARTESIAN_POINT ( 'NONE',  ( -2.179377348189611929, -71.14547149457074227, -7.030887037049939003 ) ) ;
#429 =( NAMED_UNIT ( * ) SI_UNIT ( $, .STERADIAN. ) SOLID_ANGLE_UNIT ( ) );
#430 = CARTESIAN_POINT ( 'NONE',  ( 4.460500007776900588, -96.99999999999960210, 2.535776773627464564 ) ) ;
#431 = CARTESIAN_POINT ( 'NONE',  ( 3.015831842038148025, -70.69547149457073942, -3.989209796945492048 ) ) ;
#432 = CARTESIAN_POINT ( 'NONE',  ( -4.312004677470993919, -72.04547149457074795, 3.009306630940933758 ) ) ;
#433 = CARTESIAN_POINT ( 'NONE',  ( -1.719659006605374962, -57.15452850542924068, -4.969112962950016588 ) ) ;
#434 = DIRECTION ( 'NONE',  ( 0.000000000000000000, 0.000000000000000000, -1.000000000000000000 ) ) ;
#435 = CIRCLE ( 'NONE', #50, 5.000000000000004441 ) ;
#436 = CARTESIAN_POINT ( 'NONE',  ( 0.09506052544085857869, -64.50452850542926342, 4.999999999999997335 ) ) ;
#437 = CARTESIAN_POINT ( 'NONE',  ( 4.312004677471010794, -64.54547149457073374, -3.009306630940933314 ) ) ;
#438 = EDGE_CURVE ( 'NONE', #4154, #6969, #4010, .T. ) ;
#439 = CARTESIAN_POINT ( 'NONE',  ( -4.194503406049314265, -94.05452850542926058, 3.171033256558100533 ) ) ;
#440 = ORIENTED_EDGE ( 'NONE', *, *, #4555, .F. ) ;
#441 = DIRECTION ( 'NONE',  ( -0.09506052544079829358, 0.9954714945707483498, 0.000000000000000000 ) ) ;
#442 = EDGE_LOOP ( 'NONE', ( #7113, #2192, #7963, #2069 ) ) ;
#443 = CARTESIAN_POINT ( 'NONE',  ( 50.00000000000000000, -9.999999999999994671, -1.500000000000000666 ) ) ;
#444 = CARTESIAN_POINT ( 'NONE',  ( -1.529537955723669684, -82.35452850542922931, 5.030887037049979860 ) ) ;
#445 = CARTESIAN_POINT ( 'NONE',  ( 4.725907263620374721, -94.09547149457074511, 1.635492904037598283 ) ) ;
#446 = CARTESIAN_POINT ( 'NONE',  ( 3.015831842038231958, -61.80452850542926058, 3.989209796945429432 ) ) ;
#447 = CARTESIAN_POINT ( 'NONE',  ( -1.686450176301616199, -83.29547149457074795, -2.482926158054096000 ) ) ;
#448 = CARTESIAN_POINT ( 'NONE',  ( 4.784657899331178577, -85.39547149457074227, -1.454677039711874009 ) ) ;
#449 = CARTESIAN_POINT ( 'NONE',  ( 4.194503406049335581, -71.55452850542926058, -3.171033256558100089 ) ) ;
#450 = CARTESIAN_POINT ( 'NONE',  ( 2.179377348189481811, -74.85452850542925773, -7.030887037049986077 ) ) ;
#451 = MECHANICAL_DESIGN_GEOMETRIC_PRESENTATION_REPRESENTATION (  '', ( #5824 ), #5564 ) ;
#452 = AXIS2_PLACEMENT_3D ( 'NONE', #3365, #5291, #5925 ) ;
#453 = VECTOR ( 'NONE', #2497, 1000.000000000000000 ) ;
#454 = CARTESIAN_POINT ( 'NONE',  ( -0.09506052544082121969, -60.00452850542925631, -2.999999999999997780 ) ) ;
#455 = EDGE_LOOP ( 'NONE', ( #5527, #7887, #7984, #6188 ) ) ;
#456 = LINE ( 'NONE', #3663, #5763 ) ;
#457 = AXIS2_PLACEMENT_3D ( 'NONE', #229, #7354, #5285 ) ;
#458 = EDGE_LOOP ( 'NONE', ( #2051, #7413, #7304, #5700 ) ) ;
#459 = CARTESIAN_POINT ( 'NONE',  ( 0.09506052544086197875, -91.50452850542924921, 4.999999999999997335 ) ) ;
#460 = CARTESIAN_POINT ( 'NONE',  ( -2.493201789345253161, -70.05452850542926058, 1.934965279058294518 ) ) ;
#461 = CARTESIAN_POINT ( 'NONE',  ( 5.895805022753402902, -59.55452850542924637, -4.407101234057908989 ) ) ;
#462 = CARTESIAN_POINT ( 'NONE',  ( -5.895805022753476621, -83.44547149457073942, -4.407101234057782868 ) ) ;
#463 = CARTESIAN_POINT ( 'NONE',  ( 54.99999999999999289, -19.99999999999999645, -12.50000000000000355 ) ) ;
#464 = CARTESIAN_POINT ( 'NONE',  ( -4.312004677470992142, -87.04547149457074795, 3.009306630940933314 ) ) ;
#465 = CARTESIAN_POINT ( 'NONE',  ( -1.069819614139537078, -87.15452850542926910, -2.969112962950023249 ) ) ;
#466 = PLANE ( 'NONE',  #7665 ) ;
#467 = ORIENTED_EDGE ( 'NONE', *, *, #5724, .F. ) ;
#468 =( NAMED_UNIT ( * ) PLANE_ANGLE_UNIT ( ) SI_UNIT ( $, .RADIAN. ) );
#469 = CARTESIAN_POINT ( 'NONE',  ( -0.09506052544081666777, -96.00452850542926342, -2.999999999999997780 ) ) ;
#470 = CARTESIAN_POINT ( 'NONE',  ( -7.360235569667858968, -71.74547149457075079, -0.09995255151716124498 ) ) ;
#471 = FILL_AREA_STYLE ('',( #4980 ) ) ;
#472 = CARTESIAN_POINT ( 'NONE',  ( 5.713289348668859624, -96.99999999999995737, -0.5550645300988114039 ) ) ;
#473 = CARTESIAN_POINT ( 'NONE',  ( 4.725907263620372056, -67.09547149457073090, 1.635492904037598283 ) ) ;
#474 = CARTESIAN_POINT ( 'NONE',  ( -4.725907263620354293, -71.59547149457074511, -1.635492904037597617 ) ) ;
#475 = CARTESIAN_POINT ( 'NONE',  ( -5.257311121191324155, -60.75452850542925631, 0.09995255151729526277 ) ) ;
#476 = LINE ( 'NONE', #8193, #724 ) ;
#477 = ADVANCED_FACE ( 'NONE', ( #88 ), #7132, .F. ) ;
#478 = CARTESIAN_POINT ( 'NONE',  ( -1.529537955723671239, -70.35452850542925773, 5.030887037049979860 ) ) ;
#479 = CARTESIAN_POINT ( 'NONE',  ( 4.784657899331175912, -64.39547149457074227, -1.454677039711874009 ) ) ;
#480 = VERTEX_POINT ( 'NONE', #1359 ) ;
#481 = PLANE ( 'NONE',  #6922 ) ;
#482 = ORIENTED_EDGE ( 'NONE', *, *, #2370, .T. ) ;
#483 = LINE ( 'NONE', #2313, #180 ) ;
#484 = CARTESIAN_POINT ( 'NONE',  ( 4.194503406049337357, -77.55452850542926058, -3.171033256558100089 ) ) ;
#485 = CARTESIAN_POINT ( 'NONE',  ( -1.719659006605263940, -93.34547149457071669, 4.969112962950051227 ) ) ;
#486 = CARTESIAN_POINT ( 'NONE',  ( 4.194503406049335581, -62.55452850542925347, -3.171033256558100977 ) ) ;
#487 = CARTESIAN_POINT ( 'NONE',  ( -2.882544866740858414, -68.89547149457074227, 0.8366430509619596778 ) ) ;
#488 = CARTESIAN_POINT ( 'NONE',  ( -4.191402346623179120, -75.30452850542926058, -5.607243785695311900 ) ) ;
#489 = CARTESIAN_POINT ( 'NONE',  ( 4.725907263620373833, -85.09547149457074511, 1.635492904037598283 ) ) ;
#490 = CARTESIAN_POINT ( 'NONE',  ( -4.725907263620322318, -69.90452850542925489, 1.635492904037698647 ) ) ;
#491 = CARTESIAN_POINT ( 'NONE',  ( 2.369498399071225503, -79.65452850542925489, 6.969112962950009482 ) ) ;
#492 = CARTESIAN_POINT ( 'NONE',  ( 0.8796985632579631398, -87.64547149457075648, 3.030887037049952326 ) ) ;
#493 = ORIENTED_EDGE ( 'NONE', *, *, #657, .F. ) ;
#494 = LINE ( 'NONE', #4888, #7793 ) ;
#495 = DIRECTION ( 'NONE',  ( -1.000000000000000000, -0.000000000000000000, -0.000000000000000000 ) ) ;
#496 = ORIENTED_EDGE ( 'NONE', *, *, #8064, .T. ) ;
#497 = CARTESIAN_POINT ( 'NONE',  ( -1.529537955723668796, -88.35452850542925773, 5.030887037049979860 ) ) ;
#498 = CARTESIAN_POINT ( 'NONE',  ( 1.840261337453269919, -70.80452850542926058, 2.371175808195547852 ) ) ;
#499 = VECTOR ( 'NONE', #7220, 1000.000000000000000 ) ;
#500 = CARTESIAN_POINT ( 'NONE',  ( 0.09506052544086197875, -91.50452850542924921, 4.999999999999997335 ) ) ;
#501 = CARTESIAN_POINT ( 'NONE',  ( 5.895805022753492608, -69.94547149457073942, 4.407101234057782868 ) ) ;
#502 = CARTESIAN_POINT ( 'NONE',  ( 4.784657899331178577, -82.39547149457074227, -1.454677039711874009 ) ) ;
#503 = CARTESIAN_POINT ( 'NONE',  ( 1.069819614139557284, -79.65452850542925489, 2.969112962950023249 ) ) ;
#504 = FACE_OUTER_BOUND ( 'NONE', #5035, .T. ) ;
#505 = ORIENTED_EDGE ( 'NONE', *, *, #407, .F. ) ;
#506 = CARTESIAN_POINT ( 'NONE',  ( 1.719659006605388507, -61.65452850542923358, 4.969112962950016588 ) ) ;
#507 = CARTESIAN_POINT ( 'NONE',  ( -6.013306294175060351, -75.04547149457074795, 4.245374608440741326 ) ) ;
#508 = EDGE_CURVE ( 'NONE', #4394, #4928, #3928, .T. ) ;
#509 =( NAMED_UNIT ( * ) PLANE_ANGLE_UNIT ( ) SI_UNIT ( $, .RADIAN. ) );
#510 = CARTESIAN_POINT ( 'NONE',  ( 50.00000000000000000, -12.00000000000000711, 12.49999999999999822 ) ) ;
#511 = CARTESIAN_POINT ( 'NONE',  ( 0.09506052544075412059, -67.99547149457075079, -4.999999999999997335 ) ) ;
#512 = CARTESIAN_POINT ( 'NONE',  ( 6.628020296210689111, -94.09547149457074511, 2.253526892787472757 ) ) ;
#513 = CARTESIAN_POINT ( 'NONE',  ( 2.823794231030042567, -95.40452850542926910, -1.017458915287783316 ) ) ;
#514 = CARTESIAN_POINT ( 'NONE',  ( 80.00000000000000000, -7.999999999999992895, -12.50000000000000178 ) ) ;
#515 = CIRCLE ( 'NONE', #4553, 1.500000000000000666 ) ;
#516 = CARTESIAN_POINT ( 'NONE',  ( 5.257311121191341918, -65.25452850542926342, -0.09995255151729465215 ) ) ;
#517 = CARTESIAN_POINT ( 'NONE',  ( 1.719659006605283924, -64.84547149457071669, -4.969112962950050338 ) ) ;
#518 = SURFACE_STYLE_USAGE ( .BOTH. , #4233 ) ;
#519 = ORIENTED_EDGE ( 'NONE', *, *, #6332, .T. ) ;
#520 = EDGE_CURVE ( 'NONE', #5844, #1714, #3390, .T. ) ;
#521 = AXIS2_PLACEMENT_3D ( 'NONE', #5224, #627, #804 ) ;
#522 = AXIS2_PLACEMENT_3D ( 'NONE', #3905, #2648, #1459 ) ;
#523 = DIRECTION ( 'NONE',  ( 1.000000000000000000, 0.000000000000000000, 0.000000000000000000 ) ) ;
#524 = VERTEX_POINT ( 'NONE', #5948 ) ;
#525 = DIRECTION ( 'NONE',  ( 1.261617073437677752E-16, -1.000000000000000000, -0.000000000000000000 ) ) ;
#526 = CARTESIAN_POINT ( 'NONE',  ( -4.194503406049316041, -79.05452850542921794, 3.171033256558100533 ) ) ;
#527 = EDGE_CURVE ( 'NONE', #6149, #6264, #3180, .T. ) ;
#528 = CARTESIAN_POINT ( 'NONE',  ( 4.194503406049402194, -90.94547149457071100, 3.171033256558012159 ) ) ;
#529 = CARTESIAN_POINT ( 'NONE',  ( 4.312004677471074743, -61.95452850542925205, 3.009306630940844052 ) ) ;
#530 = CARTESIAN_POINT ( 'NONE',  ( -1.686450176301617976, -68.29547149457073374, -2.482926158054096000 ) ) ;
#531 = CARTESIAN_POINT ( 'NONE',  ( 6.686770931921523164, -77.10452850542924352, 2.072711028461649008 ) ) ;
#532 = CARTESIAN_POINT ( 'NONE',  ( -4.784657899331157260, -86.89547149457074227, 1.454677039711874675 ) ) ;
#533 = CARTESIAN_POINT ( 'NONE',  ( 2.862020680886513180, -68.70452850542925205, -4.100960146804039752 ) ) ;
#534 = VECTOR ( 'NONE', #7295, 1000.000000000000000 ) ;
#535 = CARTESIAN_POINT ( 'NONE',  ( -7.360235569667858968, -75.75452850542926342, 0.09995255151731782806 ) ) ;
#536 = CARTESIAN_POINT ( 'NONE',  ( 2.493201789345310893, -84.94547149457073942, 1.934965279058241006 ) ) ;
#537 = ORIENTED_EDGE ( 'NONE', *, *, #4750, .F. ) ;
#538 = CARTESIAN_POINT ( 'NONE',  ( 43.45299461620744097, 100.0000000000000000, -7.500000000000000000 ) ) ;
#539 = DIRECTION ( 'NONE',  ( -1.000000000000000000, 0.000000000000000000, 0.000000000000000000 ) ) ;
#540 = VERTEX_POINT ( 'NONE', #5837 ) ;
#541 = CARTESIAN_POINT ( 'NONE',  ( 0.09506052544086160405, -88.50452850542924921, 4.999999999999997335 ) ) ;
#542 = CARTESIAN_POINT ( 'NONE',  ( 0.8796985632578971925, -62.85452850542923642, -3.030887037049972310 ) ) ;
#543 = ADVANCED_FACE ( 'NONE', ( #3277 ), #2060, .T. ) ;
#544 = CARTESIAN_POINT ( 'NONE',  ( -2.862020680886492308, -94.20452850542926626, 4.100960146804039752 ) ) ;
#545 = CARTESIAN_POINT ( 'NONE',  ( 7.360235569667877620, -67.24547149457075079, 0.09995255151716216091 ) ) ;
#546 = CARTESIAN_POINT ( 'NONE',  ( -0.09506052544073390065, -87.49547149457075079, 4.999999999999997335 ) ) ;
#547 = CARTESIAN_POINT ( 'NONE',  ( -2.610703060766965677, -72.45452850542925205, -1.773238653441072232 ) ) ;
#548 = PLANE ( 'NONE',  #3363 ) ;
#549 = VERTEX_POINT ( 'NONE', #4695 ) ;
#550 = DIRECTION ( 'NONE',  ( 0.000000000000000000, 0.000000000000000000, -1.000000000000000000 ) ) ;
#551 = CARTESIAN_POINT ( 'NONE',  ( 1.686450176301586223, -83.70452850542925205, -2.482926158054133303 ) ) ;
#552 = CARTESIAN_POINT ( 'NONE',  ( 7.360235569667877620, -67.24547149457075079, 0.09995255151716216091 ) ) ;
#553 = CARTESIAN_POINT ( 'NONE',  ( 1.766089183626466941, -96.99999999999998579, -5.729544030250906417 ) ) ;
#554 = CARTESIAN_POINT ( 'NONE',  ( 5.257311121191341030, -67.24547149457075079, 0.09995255151718437925 ) ) ;
#555 = CARTESIAN_POINT ( 'NONE',  ( -5.895805022753475733, -95.44547149457075363, -4.407101234057782868 ) ) ;
#556 = CARTESIAN_POINT ( 'NONE',  ( 2.493201789345274033, -95.55452850542926058, -1.934965279058294518 ) ) ;
#557 = LINE ( 'NONE', #3220, #3294 ) ;
#558 = CARTESIAN_POINT ( 'NONE',  ( 0.09506052544085932809, -70.50452850542926342, 4.999999999999997335 ) ) ;
#559 = CARTESIAN_POINT ( 'NONE',  ( 3.015831842038146693, -61.69547149457073942, -3.989209796945492048 ) ) ;
#560 = FILL_AREA_STYLE ('',( #6421 ) ) ;
#561 = ORIENTED_EDGE ( 'NONE', *, *, #611, .F. ) ;
#562 = LINE ( 'NONE', #3139, #7733 ) ;
#563 = PRODUCT_DEFINITION_SHAPE ( 'NONE', 'NONE',  #5357 ) ;
#564 = APPLICATION_PROTOCOL_DEFINITION ( 'draft international standard', 'automotive_design', 1998, #712 ) ;
#565 = EDGE_LOOP ( 'NONE', ( #768, #2129, #3059, #5475 ) ) ;
#566 = FACE_BOUND ( 'NONE', #6041, .T. ) ;
#567 = CARTESIAN_POINT ( 'NONE',  ( -2.862020680886494528, -76.20452850542926626, 4.100960146804039752 ) ) ;
#568 = CARTESIAN_POINT ( 'NONE',  ( -1.719659006605264384, -87.34547149457074511, 4.969112962950051227 ) ) ;
#569 = CARTESIAN_POINT ( 'NONE',  ( 0.09506052544085857869, -64.50452850542926342, 4.999999999999997335 ) ) ;
#570 = CARTESIAN_POINT ( 'NONE',  ( -1.069819614139475794, -69.34547149457073090, 2.969112962950044121 ) ) ;
#571 = CARTESIAN_POINT ( 'NONE',  ( -2.179377348189460939, -82.35452850542927195, 7.030887037049988741 ) ) ;
#572 = CARTESIAN_POINT ( 'NONE',  ( 5.257311121191342806, -88.24547149457073658, 0.09995255151718437925 ) ) ;
#573 = CARTESIAN_POINT ( 'NONE',  ( 75.00000000000000000, -9.999999999999994671, 1.500000000000000666 ) ) ;
#574 = CARTESIAN_POINT ( 'NONE',  ( 2.369498399071225059, -76.65452850542925489, 6.969112962950009482 ) ) ;
#575 = CARTESIAN_POINT ( 'NONE',  ( -2.882544866740856637, -86.89547149457074227, 0.8366430509619596778 ) ) ;
#576 = EDGE_CURVE ( 'NONE', #1381, #2388, #1975, .T. ) ;
#577 = VERTEX_POINT ( 'NONE', #7832 ) ;
#578 = LINE ( 'NONE', #2656, #3221 ) ;
#579 = CARTESIAN_POINT ( 'NONE',  ( 75.00000000000000000, -20.00000000000000000, -7.500000000000000000 ) ) ;
#580 = ORIENTED_EDGE ( 'NONE', *, *, #1489, .F. ) ;
#581 = CARTESIAN_POINT ( 'NONE',  ( 4.312004677471078296, -88.95452850542925205, 3.009306630940844052 ) ) ;
#582 = CARTESIAN_POINT ( 'NONE',  ( -1.840261337453253931, -60.30452850542926058, -2.371175808195547852 ) ) ;
#583 = EDGE_CURVE ( 'NONE', #2431, #1587, #151, .T. ) ;
#584 = CARTESIAN_POINT ( 'NONE',  ( -7.360235569667860744, -57.75452850542924921, 0.09995255151731782806 ) ) ;
#585 = VECTOR ( 'NONE', #4039, 1000.000000000000000 ) ;
#586 = CARTESIAN_POINT ( 'NONE',  ( -7.360235569667860744, -65.74547149457073658, -0.09995255151716124498 ) ) ;
#587 = CARTESIAN_POINT ( 'NONE',  ( 4.725907263620374721, -91.09547149457074511, 1.635492904037598283 ) ) ;
#588 = CARTESIAN_POINT ( 'NONE',  ( -1.840261337453252155, -72.30452850542926058, -2.371175808195547852 ) ) ;
#589 = AXIS2_PLACEMENT_3D ( 'NONE', #100, #733, #2054 ) ;
#590 = DIRECTION ( 'NONE',  ( 1.000000000000000000, 0.000000000000000000, 0.000000000000000000 ) ) ;
#591 = DIRECTION ( 'NONE',  ( -1.000000000000000000, -0.000000000000000000, -0.000000000000000000 ) ) ;
#592 = CARTESIAN_POINT ( 'NONE',  ( -1.840261337453250157, -87.30452850542926058, -2.371175808195547852 ) ) ;
#593 = CARTESIAN_POINT ( 'NONE',  ( -0.09506052544071605381, -60.49547149457073658, 6.999999999999997335 ) ) ;
#594 = CARTESIAN_POINT ( 'NONE',  ( -80.00000000000000000, 2.168404344971008868E-15, -12.50000000000000000 ) ) ;
#595 = CARTESIAN_POINT ( 'NONE',  ( 4.725907263620371168, -64.09547149457073090, 1.635492904037598283 ) ) ;
#596 = CARTESIAN_POINT ( 'NONE',  ( 0.09506052544075337118, -61.99547149457074369, -4.999999999999997335 ) ) ;
#597 = CARTESIAN_POINT ( 'NONE',  ( 0.8796985632579009673, -92.85452850542924352, -3.030887037049972310 ) ) ;
#598 = DIRECTION ( 'NONE',  ( -1.000000000000000000, -0.000000000000000000, -0.000000000000000000 ) ) ;
#599 = CARTESIAN_POINT ( 'NONE',  ( 4.194503406049335581, -65.55452850542923215, -3.171033256558100089 ) ) ;
#600 = CARTESIAN_POINT ( 'NONE',  ( -5.895805022753476621, -89.44547149457073942, -4.407101234057782868 ) ) ;
#601 = EDGE_LOOP ( 'NONE', ( #1616, #6343 ) ) ;
#602 = EDGE_CURVE ( 'NONE', #5645, #577, #5831, .T. ) ;
#603 = CARTESIAN_POINT ( 'NONE',  ( -6.000000000000007994, -51.00000000000000711, -2.499999999999999112 ) ) ;
#604 = VERTEX_POINT ( 'NONE', #826 ) ;
#605 = CARTESIAN_POINT ( 'NONE',  ( 43.45299461620743386, 65.00000000000000000, 7.500000000000000000 ) ) ;
#606 = CARTESIAN_POINT ( 'NONE',  ( 1.719659006605391394, -79.65452850542925489, 4.969112962950016588 ) ) ;
#607 = CARTESIAN_POINT ( 'NONE',  ( 4.784657899331177688, -76.39547149457074227, -1.454677039711874009 ) ) ;
#608 = CARTESIAN_POINT ( 'NONE',  ( 4.227364539074073946, -96.99999999999998579, -0.5958093000394333316 ) ) ;
#609 = CARTESIAN_POINT ( 'NONE',  ( -2.882544866740858414, -71.89547149457074227, 0.8366430509619596778 ) ) ;
#610 = CARTESIAN_POINT ( 'NONE',  ( -4.037591185471422150, -82.20452850542925205, 5.718994135553947977 ) ) ;
#611 = EDGE_CURVE ( 'NONE', #5740, #6524, #3988, .T. ) ;
#612 = CARTESIAN_POINT ( 'NONE',  ( 5.257311121191341918, -85.24547149457075079, 0.09995255151718437925 ) ) ;
#613 = CARTESIAN_POINT ( 'NONE',  ( -80.00000000000000000, -25.00000000000000000, 20.00000000000000000 ) ) ;
#614 = CARTESIAN_POINT ( 'NONE',  ( 4.725907263620342746, -95.40452850542925489, -1.635492904037697981 ) ) ;
#615 = CARTESIAN_POINT ( 'NONE',  ( -2.369498399071206407, -81.15452850542924068, -6.969112962950009482 ) ) ;
#616 = CARTESIAN_POINT ( 'NONE',  ( 0.8796985632579628067, -84.64547149457074227, 3.030887037049952326 ) ) ;
#617 = ORIENTED_EDGE ( 'NONE', *, *, #2035, .T. ) ;
#618 = FACE_OUTER_BOUND ( 'NONE', #620, .T. ) ;
#619 = CARTESIAN_POINT ( 'NONE',  ( -47.50000000000000711, -97.00000000000000000, 12.49999999999993960 ) ) ;
#620 = EDGE_LOOP ( 'NONE', ( #5338, #2831, #6955, #4736 ) ) ;
#621 = CARTESIAN_POINT ( 'NONE',  ( 4.194503406049339134, -83.55452850542924637, -3.171033256558100977 ) ) ;
#622 = CARTESIAN_POINT ( 'NONE',  ( -2.882544866740879730, -57.60452850542926484, -0.8366430509618996147 ) ) ;
#623 = CARTESIAN_POINT ( 'NONE',  ( -4.037591185471424815, -61.20452850542925916, 5.718994135553947977 ) ) ;
#624 = CARTESIAN_POINT ( 'NONE',  ( -2.179377348189611929, -71.14547149457074227, -7.030887037049939003 ) ) ;
#625 = CARTESIAN_POINT ( 'NONE',  ( -4.784657899331157260, -83.89547149457074227, 1.454677039711874675 ) ) ;
#626 = CARTESIAN_POINT ( 'NONE',  ( 1.069819614139557062, -76.65452850542925489, 2.969112962950023249 ) ) ;
#627 = DIRECTION ( 'NONE',  ( -0.000000000000000000, -0.000000000000000000, -1.000000000000000000 ) ) ;
#628 = CARTESIAN_POINT ( 'NONE',  ( 80.00000000000000000, 0.000000000000000000, 20.00000000000000000 ) ) ;
#629 = CARTESIAN_POINT ( 'NONE',  ( 0.09506052544083994083, -85.50452850542926342, 2.999999999999997780 ) ) ;
#630 = CARTESIAN_POINT ( 'NONE',  ( 5.895805022753492608, -63.94547149457074653, 4.407101234057782868 ) ) ;
#631 = DIRECTION ( 'NONE',  ( -1.000000000000000000, -9.251858538542971581E-17, 0.000000000000000000 ) ) ;
#632 = CARTESIAN_POINT ( 'NONE',  ( 2.862020680886598889, -69.79547149457074795, 4.100960146803977580 ) ) ;
#633 = CARTESIAN_POINT ( 'NONE',  ( -4.194503406049384431, -62.44547149457072521, -3.171033256558012159 ) ) ;
#634 = LINE ( 'NONE', #6416, #4270 ) ;
#635 = ADVANCED_FACE ( 'NONE', ( #7236 ), #3406, .F. ) ;
#636 = LINE ( 'NONE', #5776, #2593 ) ;
#637 = AXIS2_PLACEMENT_3D ( 'NONE', #2916, #7427, #1567 ) ;
#638 = CARTESIAN_POINT ( 'NONE',  ( -0.09506052544084186984, -63.00452850542925631, -4.999999999999997335 ) ) ;
#639 = CARTESIAN_POINT ( 'NONE',  ( -0.09506052544071189048, -93.49547149457075079, 6.999999999999997335 ) ) ;
#640 =( NAMED_UNIT ( * ) PLANE_ANGLE_UNIT ( ) SI_UNIT ( $, .RADIAN. ) );
#641 = ORIENTED_EDGE ( 'NONE', *, *, #1752, .T. ) ;
#642 = CARTESIAN_POINT ( 'NONE',  ( -4.725907263620321430, -72.90452850542925489, 1.635492904037698647 ) ) ;
#643 = LINE ( 'NONE', #7606, #1269 ) ;
#644 = PLANE ( 'NONE',  #1398 ) ;
#645 = CARTESIAN_POINT ( 'NONE',  ( 4.312004677471013459, -82.54547149457074795, -3.009306630940933314 ) ) ;
#646 = VECTOR ( 'NONE', #7811, 1000.000000000000000 ) ;
#647 = FACE_OUTER_BOUND ( 'NONE', #5300, .T. ) ;
#648 = CARTESIAN_POINT ( 'NONE',  ( 3.154386672714808437, -73.24547149457075079, 0.09995255151720662534 ) ) ;
#649 = VECTOR ( 'NONE', #4755, 1000.000000000000000 ) ;
#650 = CARTESIAN_POINT ( 'NONE',  ( 6.013306294175169597, -73.95452850542925205, 4.245374608440616093 ) ) ;
#651 = CARTESIAN_POINT ( 'NONE',  ( -3.015831842038128929, -78.19547149457075363, 3.989209796945492048 ) ) ;
#652 = CARTESIAN_POINT ( 'NONE',  ( -2.862020680886496304, -61.20452850542925205, 4.100960146804039752 ) ) ;
#653 = CARTESIAN_POINT ( 'NONE',  ( 43.45299461620743386, 65.00000000000000000, 7.500000000000000000 ) ) ;
#654 = CARTESIAN_POINT ( 'NONE',  ( -0.09506052544086177059, -72.00452850542926342, -6.999999999999997335 ) ) ;
#655 = VECTOR ( 'NONE', #3803, 1000.000000000000000 ) ;
#656 = CARTESIAN_POINT ( 'NONE',  ( -0.8796985632579414904, -89.14547149457072805, -3.030887037049952326 ) ) ;
#657 = EDGE_CURVE ( 'NONE', #72, #1757, #1333, .T. ) ;
#658 = ORIENTED_EDGE ( 'NONE', *, *, #657, .T. ) ;
#659 = FACE_BOUND ( 'NONE', #6052, .T. ) ;
#660 = DIRECTION ( 'NONE',  ( -0.000000000000000000, -0.000000000000000000, -1.000000000000000000 ) ) ;
#661 = CARTESIAN_POINT ( 'NONE',  ( -4.312004677471056979, -84.45452850542922363, -3.009306630940844052 ) ) ;
#662 = EDGE_LOOP ( 'NONE', ( #2589, #4451, #6768, #2881 ) ) ;
#663 = CARTESIAN_POINT ( 'NONE',  ( -5.257311121191323267, -84.75452850542924921, 0.09995255151729529053 ) ) ;
#664 = CARTESIAN_POINT ( 'NONE',  ( -2.610703060766967454, -57.45452850542925916, -1.773238653441072232 ) ) ;
#665 = CIRCLE ( 'NONE', #6993, 1.500000000000001776 ) ;
#666 = DIRECTION ( 'NONE',  ( 0.000000000000000000, 0.000000000000000000, 1.000000000000000000 ) ) ;
#667 = CARTESIAN_POINT ( 'NONE',  ( -1.529537955723668574, -88.35452850542925773, 5.030887037049979860 ) ) ;
#668 = CARTESIAN_POINT ( 'NONE',  ( -0.09506052544071454113, -72.49547149457075079, 6.999999999999997335 ) ) ;
#669 = EDGE_CURVE ( 'NONE', #1798, #1772, #3320, .T. ) ;
#670 = CARTESIAN_POINT ( 'NONE',  ( 0.09506052544075563326, -79.99547149457075079, -4.999999999999997335 ) ) ;
#671 = CARTESIAN_POINT ( 'NONE',  ( -2.493201789345252717, -73.05452850542926058, 1.934965279058294518 ) ) ;
#672 =( GEOMETRIC_REPRESENTATION_CONTEXT ( 3 ) GLOBAL_UNCERTAINTY_ASSIGNED_CONTEXT ( ( #2169 ) ) GLOBAL_UNIT_ASSIGNED_CONTEXT ( ( #902, #4727, #5913 ) ) REPRESENTATION_CONTEXT ( 'NONE', 'WORKASPACE' ) );
#673 = FACE_OUTER_BOUND ( 'NONE', #163, .T. ) ;
#674 = VECTOR ( 'NONE', #2142, 1000.000000000000000 ) ;
#675 = CARTESIAN_POINT ( 'NONE',  ( 50.00000000000000000, -20.00000000000000355, 12.49999999999999645 ) ) ;
#676 = CARTESIAN_POINT ( 'NONE',  ( 0.09506052544084032940, -88.50452850542926342, 2.999999999999997780 ) ) ;
#677 = CARTESIAN_POINT ( 'NONE',  ( 6.013306294175077227, -61.54547149457074084, -4.245374608440741326 ) ) ;
#678 = CARTESIAN_POINT ( 'NONE',  ( 40.00000000000000000, -9.999999999999991118, 9.499999999999998224 ) ) ;
#679 = CARTESIAN_POINT ( 'NONE',  ( -4.784657899331190123, -72.60452850542925773, -1.454677039711773867 ) ) ;
#680 = CARTESIAN_POINT ( 'NONE',  ( 6.628020296210689999, -97.09547149457074511, 2.253526892787472757 ) ) ;
#681 = CARTESIAN_POINT ( 'NONE',  ( -80.00000000000000000, 2.168404344971008868E-15, -12.50000000000000000 ) ) ;
#682 = CARTESIAN_POINT ( 'NONE',  ( 6.000000000000006217, -51.00000000000000711, -2.499999999999999112 ) ) ;
#683 = CARTESIAN_POINT ( 'NONE',  ( -3.015831842038217303, -57.30452850542925347, -3.989209796945429432 ) ) ;
#684 = CARTESIAN_POINT ( 'NONE',  ( -6.686770931921456551, -92.89547149457074227, 2.072711028461789784 ) ) ;
#685 = EDGE_LOOP ( 'NONE', ( #7292, #5717, #2988, #1427 ) ) ;
#686 = CARTESIAN_POINT ( 'NONE',  ( 4.784657899331209663, -74.10452850542925773, 1.454677039711774533 ) ) ;
#687 = CARTESIAN_POINT ( 'NONE',  ( 80.00000000000000000, -25.00000000000000000, 20.00000000000000000 ) ) ;
#688 = CARTESIAN_POINT ( 'NONE',  ( -47.50000000000000711, -46.99999999999998579, -12.50000000000000888 ) ) ;
#689 = CARTESIAN_POINT ( 'NONE',  ( -2.862020680886579793, -83.29547149457074795, -4.100960146803977580 ) ) ;
#690 = CARTESIAN_POINT ( 'NONE',  ( -1.500000000000000666, -26.99999999999998934, -7.000000000000000000 ) ) ;
#691 = CARTESIAN_POINT ( 'NONE',  ( -2.882544866740859302, -65.89547149457074227, 0.8366430509619596778 ) ) ;
#692 = CARTESIAN_POINT ( 'NONE',  ( -6.628020296210622497, -66.90452850542925489, 2.253526892787613978 ) ) ;
#693 = DIRECTION ( 'NONE',  ( 0.000000000000000000, 0.000000000000000000, 1.000000000000000000 ) ) ;
#694 = EDGE_CURVE ( 'NONE', #3832, #7792, #3206, .T. ) ;
#695 = CARTESIAN_POINT ( 'NONE',  ( -4.312004677470993030, -78.04547149457076216, 3.009306630940933758 ) ) ;
#696 = CARTESIAN_POINT ( 'NONE',  ( -3.015831842038216859, -60.30452850542926058, -3.989209796945429432 ) ) ;
#697 = CARTESIAN_POINT ( 'NONE',  ( 4.784657899331212327, -95.10452850542925773, 1.454677039711774533 ) ) ;
#698 = CARTESIAN_POINT ( 'NONE',  ( 0.09506052544087986722, -64.50452850542926342, 6.999999999999997335 ) ) ;
#699 = CARTESIAN_POINT ( 'NONE',  ( -1.069819614139474240, -81.34547149457074511, 2.969112962950044121 ) ) ;
#700 = AXIS2_PLACEMENT_3D ( 'NONE', #5107, #2634, #5148 ) ;
#701 = ORIENTED_EDGE ( 'NONE', *, *, #4023, .T. ) ;
#702 = CARTESIAN_POINT ( 'NONE',  ( -5.999999999999993783, -47.00000000000000000, -2.499999999999999112 ) ) ;
#703 = DIRECTION ( 'NONE',  ( -1.000000000000000000, -0.000000000000000000, -0.000000000000000000 ) ) ;
#704 = CARTESIAN_POINT ( 'NONE',  ( 1.719659006605392504, -88.65452850542925489, 4.969112962950016588 ) ) ;
#705 = ORIENTED_EDGE ( 'NONE', *, *, #1358, .T. ) ;
#706 = CARTESIAN_POINT ( 'NONE',  ( -1.529537955723669684, -82.35452850542924352, 5.030887037049979860 ) ) ;
#707 = CARTESIAN_POINT ( 'NONE',  ( -2.610703060766923933, -96.04547149457074795, 1.773238653441125745 ) ) ;
#708 = DIRECTION ( 'NONE',  ( 0.000000000000000000, 0.000000000000000000, 1.000000000000000000 ) ) ;
#709 = CARTESIAN_POINT ( 'NONE',  ( -2.862020680886492308, -91.20452850542926626, 4.100960146804039752 ) ) ;
#710 = CARTESIAN_POINT ( 'NONE',  ( -0.09506052544071567911, -63.49547149457075079, 6.999999999999997335 ) ) ;
#711 = CARTESIAN_POINT ( 'NONE',  ( -0.8796985632578805392, -67.35452850542924352, 3.030887037049973198 ) ) ;
#712 = APPLICATION_CONTEXT ( 'automotive_design' ) ;
#713 = DIRECTION ( 'NONE',  ( -0.000000000000000000, -0.000000000000000000, -1.000000000000000000 ) ) ;
#714 = LINE ( 'NONE', #5810, #3097 ) ;
#715 = CARTESIAN_POINT ( 'NONE',  ( 2.823794231030041235, -83.40452850542925489, -1.017458915287783316 ) ) ;
#716 = VECTOR ( 'NONE', #6719, 1000.000000000000000 ) ;
#717 = CARTESIAN_POINT ( 'NONE',  ( -2.179377348189612817, -62.14547149457074937, -7.030887037049939003 ) ) ;
#718 = VECTOR ( 'NONE', #2739, 1000.000000000000000 ) ;
#719 = FACE_OUTER_BOUND ( 'NONE', #1634, .T. ) ;
#720 = CARTESIAN_POINT ( 'NONE',  ( -4.784657899331190123, -75.60452850542925773, -1.454677039711773867 ) ) ;
#721 = CARTESIAN_POINT ( 'NONE',  ( -6.013306294175058575, -93.04547149457074795, 4.245374608440741326 ) ) ;
#722 = FACE_BOUND ( 'NONE', #2870, .T. ) ;
#723 = FACE_OUTER_BOUND ( 'NONE', #8185, .T. ) ;
#724 = VECTOR ( 'NONE', #4868, 1000.000000000000114 ) ;
#725 =( GEOMETRIC_REPRESENTATION_CONTEXT ( 3 ) GLOBAL_UNCERTAINTY_ASSIGNED_CONTEXT ( ( #4274 ) ) GLOBAL_UNIT_ASSIGNED_CONTEXT ( ( #2414, #6289, #2536 ) ) REPRESENTATION_CONTEXT ( 'NONE', 'WORKASPACE' ) );
#726 = EDGE_CURVE ( 'NONE', #5175, #8255, #5334, .T. ) ;
#727 = CARTESIAN_POINT ( 'NONE',  ( -5.257311121191324155, -63.75452850542925631, 0.09995255151729526277 ) ) ;
#728 = CARTESIAN_POINT ( 'NONE',  ( -5.895805022753476621, -86.44547149457073942, -4.407101234057782868 ) ) ;
#729 = CIRCLE ( 'NONE', #4630, 1.500000000000001998 ) ;
#730 = SURFACE_STYLE_USAGE ( .BOTH. , #5196 ) ;
#731 = VERTEX_POINT ( 'NONE', #4655 ) ;
#732 = CARTESIAN_POINT ( 'NONE',  ( -1.529537955723670350, -76.35452850542925773, 5.030887037049979860 ) ) ;
#733 = DIRECTION ( 'NONE',  ( 0.000000000000000000, -2.168404344971010347E-16, 1.000000000000000000 ) ) ;
#734 = EDGE_CURVE ( 'NONE', #4784, #5781, #271, .T. ) ;
#735 = DIRECTION ( 'NONE',  ( -0.000000000000000000, 0.000000000000000000, -1.000000000000000000 ) ) ;
#736 = CARTESIAN_POINT ( 'NONE',  ( -4.725907263620352516, -83.59547149457074511, -1.635492904037597617 ) ) ;
#737 = DIRECTION ( 'NONE',  ( -1.000000000000000000, 0.000000000000000000, 0.000000000000000000 ) ) ;
#738 = CARTESIAN_POINT ( 'NONE',  ( -0.09506052544075821453, -63.49547149457075079, 2.999999999999997780 ) ) ;
#739 = CARTESIAN_POINT ( 'NONE',  ( 7.360235569667877620, -71.25452850542926342, -0.09995255151731691212 ) ) ;
#740 = DIRECTION ( 'NONE',  ( 0.000000000000000000, 0.000000000000000000, -1.000000000000000000 ) ) ;
#741 = CARTESIAN_POINT ( 'NONE',  ( 4.784657899331177688, -76.39547149457074227, -1.454677039711874009 ) ) ;
#742 = CARTESIAN_POINT ( 'NONE',  ( -5.257311121191324155, -57.75452850542923500, 0.09995255151729526277 ) ) ;
#743 = CARTESIAN_POINT ( 'NONE',  ( 0.09506052544086121547, -85.50452850542926342, 4.999999999999997335 ) ) ;
#744 = CARTESIAN_POINT ( 'NONE',  ( -7.360235569667860744, -63.75452850542926342, 0.09995255151731782806 ) ) ;
#745 = CARTESIAN_POINT ( 'NONE',  ( 2.493201789345310448, -81.94547149457073942, 1.934965279058241006 ) ) ;
#746 = ORIENTED_EDGE ( 'NONE', *, *, #4954, .T. ) ;
#747 = LINE ( 'NONE', #4618, #7256 ) ;
#748 = LINE ( 'NONE', #5933, #187 ) ;
#749 = CARTESIAN_POINT ( 'NONE',  ( 4.194503406049339134, -86.55452850542926058, -3.171033256558100089 ) ) ;
#750 = ORIENTED_EDGE ( 'NONE', *, *, #6561, .T. ) ;
#751 = CARTESIAN_POINT ( 'NONE',  ( -4.784657899331190123, -84.60452850542927195, -1.454677039711773867 ) ) ;
#752 = CARTESIAN_POINT ( 'NONE',  ( 0.8796985632579640280, -93.64547149457074227, 3.030887037049952326 ) ) ;
#753 = CARTESIAN_POINT ( 'NONE',  ( 23.61234713001928753, 1.479329619654001338, 2.499999999999995115 ) ) ;
#754 = CARTESIAN_POINT ( 'NONE',  ( 4.194503406049339134, -89.55452850542926058, -3.171033256558100089 ) ) ;
#755 = CARTESIAN_POINT ( 'NONE',  ( 6.686770931921476979, -61.39547149457074937, -2.072711028461788896 ) ) ;
#756 = CARTESIAN_POINT ( 'NONE',  ( -0.8796985632578802061, -70.35452850542922931, 3.030887037049973198 ) ) ;
#757 = DIRECTION ( 'NONE',  ( 0.09506052544079829358, -0.9954714945707482388, 0.000000000000000000 ) ) ;
#758 = CARTESIAN_POINT ( 'NONE',  ( 45.00000000000000000, -15.00000000000000000, -4.163336342344337027E-15 ) ) ;
#759 = CARTESIAN_POINT ( 'NONE',  ( -2.882544866740877065, -78.60452850542927195, -0.8366430509618996147 ) ) ;
#760 = CARTESIAN_POINT ( 'NONE',  ( -5.895805022753383362, -91.05452850542926058, 4.407101234057909878 ) ) ;
#761 = DIRECTION ( 'NONE',  ( -0.000000000000000000, -0.000000000000000000, -1.000000000000000000 ) ) ;
#762 = CARTESIAN_POINT ( 'NONE',  ( -1.719659006605371854, -78.15452850542925489, -4.969112962950016588 ) ) ;
#763 = CARTESIAN_POINT ( 'NONE',  ( 2.369498399071078509, -85.84547149457074511, -6.969112962950057444 ) ) ;
#764 = DIRECTION ( 'NONE',  ( -0.000000000000000000, -2.775557561562892337E-16, 1.000000000000000000 ) ) ;
#765 = PLANE ( 'NONE',  #5548 ) ;
#766 = CARTESIAN_POINT ( 'NONE',  ( -2.882544866740858414, -71.89547149457074227, 0.8366430509619596778 ) ) ;
#767 = SURFACE_STYLE_USAGE ( .BOTH. , #2128 ) ;
#768 = ORIENTED_EDGE ( 'NONE', *, *, #6942, .T. ) ;
#769 = ADVANCED_FACE ( 'NONE', ( #1502 ), #4069, .F. ) ;
#770 = CARTESIAN_POINT ( 'NONE',  ( -3.015831842038215083, -75.30452850542926058, -3.989209796945429432 ) ) ;
#771 = CARTESIAN_POINT ( 'NONE',  ( -5.895805022753476621, -92.44547149457073942, -4.407101234057782868 ) ) ;
#772 =( LENGTH_UNIT ( ) NAMED_UNIT ( * ) SI_UNIT ( .MILLI., .METRE. ) );
#773 = EDGE_LOOP ( 'NONE', ( #701, #3537, #1533, #746 ) ) ;
#774 = VECTOR ( 'NONE', #3392, 1000.000000000000000 ) ;
#775 = CARTESIAN_POINT ( 'NONE',  ( -2.862020680886494972, -73.20452850542925205, 4.100960146804039752 ) ) ;
#776 = DIRECTION ( 'NONE',  ( -0.9954714945707483498, -0.09506052544079827971, 1.047588144072330487E-14 ) ) ;
#777 = EDGE_CURVE ( 'NONE', #3733, #7693, #19, .T. ) ;
#778 = DIRECTION ( 'NONE',  ( -0.000000000000000000, 1.000000000000000000, 1.734723475976807094E-16 ) ) ;
#779 = ADVANCED_FACE ( 'NONE', ( #5248 ), #6638, .F. ) ;
#780 = CARTESIAN_POINT ( 'NONE',  ( 0.09506052544075563326, -79.99547149457075079, -4.999999999999997335 ) ) ;
#781 = DIRECTION ( 'NONE',  ( -0.000000000000000000, -1.387778780781445676E-16, 1.000000000000000000 ) ) ;
#782 = CARTESIAN_POINT ( 'NONE',  ( -3.154386672714791118, -65.74547149457073658, -0.09995255151720625064 ) ) ;
#783 = CARTESIAN_POINT ( 'NONE',  ( 0.09506052544088025580, -67.50452850542926342, 6.999999999999997335 ) ) ;
#784 = DIRECTION ( 'NONE',  ( 1.000000000000000000, 0.000000000000000000, 0.000000000000000000 ) ) ;
#785 = CARTESIAN_POINT ( 'NONE',  ( 1.719659006605286145, -79.84547149457071669, -4.969112962950050338 ) ) ;
#786 = CARTESIAN_POINT ( 'NONE',  ( 5.257311121191341918, -83.25452850542926342, -0.09995255151729465215 ) ) ;
#787 = CARTESIAN_POINT ( 'NONE',  ( 4.191402346623196884, -67.80452850542926058, 5.607243785695311900 ) ) ;
#788 = CARTESIAN_POINT ( 'NONE',  ( 0.09506052544077704669, -82.99547149457075079, -2.999999999999997780 ) ) ;
#789 = ORIENTED_EDGE ( 'NONE', *, *, #1868, .T. ) ;
#790 = AXIS2_PLACEMENT_3D ( 'NONE', #5005, #6189, #6861 ) ;
#791 = LINE ( 'NONE', #5465, #585 ) ;
#792 = CARTESIAN_POINT ( 'NONE',  ( 47.49999999999999289, -198.2344135219424857, 12.49999999999993960 ) ) ;
#793 = CARTESIAN_POINT ( 'NONE',  ( 1.719659006605392504, -91.65452850542925489, 4.969112962950016588 ) ) ;
#794 = ORIENTED_EDGE ( 'NONE', *, *, #5429, .T. ) ;
#795 = CARTESIAN_POINT ( 'NONE',  ( 2.862020680886514956, -83.70452850542925205, -4.100960146804039752 ) ) ;
#796 = CARTESIAN_POINT ( 'NONE',  ( -0.09506052544075442590, -93.49547149457075079, 2.999999999999997780 ) ) ;
#797 =( BOUNDED_CURVE ( )  B_SPLINE_CURVE ( 2, ( #2958, #3507, #1099, #5525, #1568, #4134, #4935, #2251, #340, #1058, #6197, #7508, #6076, #8024, #422, #8105, #977, #8062, #4806, #3630, #4214, #2293, #300, #3544, #6114, #2917, #6787, #5483, #1020, #2331, #4896, #1699, #4255, #6825, #2996, #3671, #1738, #4296, #6239, #5562, #587, #5679, #5643, #1951, #6408, #1227, #2533, #2575, #7588, #7675, #5013, #4335, #6368, #3797, #4502, #5055, #1145, #2288, #7081, #5601, #6327, #3167, #5722, #1267, #546, #4973, #5136, #464, #7631, #1824, #8301, #7548, #5095, #3208, #3123, #4456, #1866, #1907, #3714, #2494, #1185, #7715, #4414, #6996, #7038, #1307, #3838, #4376, #625, #3879, #5764, #1779, #3039, #8182, #6909, #6951, #2410, #6284, #502, #3080, #8222, #2451, #3754, #8262, #5807, #6449, #36, #2622, #5182, #7761, #1992, #1351, #4541, #7124, #670, #3251, #6797, #945, #5570, #1578, #3005, #7436, #6165, #2303, #6124, #8153, #7352, #6084, #5409, #3516, #4184, #4144, #6755, #1028, #6877, #4907, #7989, #987, #4226, #6714, #2382, #390, #8033, #309, #2886, #268, #4263, #3554, #2217, #3597, #1108, #3642, #4776, #4865, #5454, #2848, #2260, #4816, #8114, #5532, #7394, #349, #6836, #1624, #2339, #2927, #5492, #1664, #8073, #6042, #4942, #2967, #1068, #7479, #1707, #6207, #431, #7516, #1747, #4305, #3049, #5687, #632, #3, #6374, #4509, #4983, #2540, #6251, #6336, #8190, #3845, #5729, #1193, #511, #4467, #8310, #3764, #2461, #554, #473, #8230, #7724, #1959, #5104, #5022, #7006, #7088, #8270, #7557, #6414, #3216, #1789, #7598, #2501, #5611, #2420, #6293, #5773, #3090, #595, #4344, #3680, #1233, #6920, #1155, #2582, #5650, #3132, #1915, #7046, #5145, #3723, #1834, #1276, #3804, #4385, #5062, #6961, #7641, #1874, #4422, #3174, #7682, #3073, #1259, #7073, #1178, #1858, #1817, #4407, #7030, #4534, #2569, #5635 ),
 .UNSPECIFIED., .F., .T. ) 
 B_SPLINE_CURVE_WITH_KNOTS ( ( 3, 2, 2, 2, 2, 2, 2, 2, 2, 2, 2, 2, 2, 2, 2, 2, 2, 2, 2, 2, 2, 2, 2, 2, 2, 2, 2, 2, 2, 2, 2, 2, 2, 2, 2, 2, 2, 2, 2, 2, 2, 2, 2, 2, 2, 2, 2, 2, 2, 2, 2, 2, 2, 2, 2, 2, 2, 2, 2, 2, 2, 2, 2, 2, 2, 2, 2, 2, 2, 2, 2, 2, 2, 2, 2, 2, 2, 2, 2, 2, 2, 2, 2, 2, 2, 2, 2, 2, 2, 2, 2, 2, 2, 2, 2, 2, 2, 2, 2, 2, 2, 2, 2, 2, 2, 2, 2, 2, 2, 2, 2, 2, 2, 2, 2, 2, 2, 2, 2, 2, 2, 2, 2, 2, 2, 2, 2, 3 ),
 ( 0.02555479535913396730, 0.03076923076923077094, 0.03846153846153846367, 0.04615384615384615641, 0.05384615384615384914, 0.06153846153846154188, 0.06923076923076923461, 0.07692307692307692735, 0.08461538461538462008, 0.09230769230769231282, 0.1000000000000000056, 0.1076923076923076983, 0.1153846153846153910, 0.1230769230769230838, 0.1307692307692307765, 0.1384615384615384692, 0.1461538461538461620, 0.1538461538461538547, 0.1615384615384615197, 0.1692307692307692402, 0.1769230769230769329, 0.1846153846153846256, 0.1923076923076923184, 0.2000000000000000111, 0.2076923076923077038, 0.2153846153846153966, 0.2230769230769230893, 0.2307692307692307820, 0.2384615384615384748, 0.2461538461538461675, 0.2538461538461538325, 0.2615384615384615530, 0.2692307692307692180, 0.2769230769230769384, 0.2846153846153846034, 0.2923076923076923239, 0.2999999999999999889, 0.3076923076923077094, 0.3153846153846153744, 0.3230769230769230949, 0.3307692307692307598, 0.3384615384615384803, 0.3461538461538461453, 0.3538461538461539213, 0.3615384615384615308, 0.3692307692307692513, 0.3769230769230769162, 0.3846153846153846367, 0.3923076923076923017, 0.4000000000000000222, 0.4076923076923076872, 0.4153846153846154077, 0.4230769230769230727, 0.4307692307692307931, 0.4384615384615384581, 0.4461538461538461786, 0.4538461538461538436, 0.4615384615384615641, 0.4692307692307692291, 0.4769230769230769496, 0.4846153846153846145, 0.4923076923076923350, 0.5000000000000000000, 0.5076923076923076650, 0.5153846153846153300, 0.5230769230769231060, 0.5307692307692307709, 0.5384615384615384359, 0.5461538461538461009, 0.5538461538461538769, 0.5615384615384615419, 0.5692307692307692069, 0.5769230769230768718, 0.5846153846153846478, 0.5923076923076923128, 0.5999999999999999778, 0.6076923076923076428, 0.6153846153846154188, 0.6230769230769230838, 0.6307692307692307487, 0.6384615384615384137, 0.6461538461538461897, 0.6538461538461538547, 0.6615384615384615197, 0.6692307692307691847, 0.6769230769230769607, 0.6846153846153846256, 0.6923076923076922906, 0.6999999999999999556, 0.7076923076923077316, 0.7153846153846153966, 0.7230769230769230616, 0.7307692307692307265, 0.7384615384615385025, 0.7461538461538461675, 0.7538461538461538325, 0.7615384615384614975, 0.7692307692307692735, 0.7769230769230769384, 0.7846153846153846034, 0.7923076923076922684, 0.8000000000000000444, 0.8076923076923077094, 0.8153846153846153744, 0.8230769230769230393, 0.8307692307692308153, 0.8384615384615384803, 0.8461538461538461453, 0.8538461538461538103, 0.8615384615384615863, 0.8692307692307692513, 0.8769230769230769162, 0.8846153846153845812, 0.8923076923076923572, 0.9000000000000000222, 0.9076923076923076872, 0.9153846153846153522, 0.9230769230769231282, 0.9307692307692307931, 0.9384615384615384581, 0.9461538461538461231, 0.9538461538461538991, 0.9615384615384615641, 0.9692307692307692291, 0.9769230769230768940, 0.9846153846153846700, 0.9923076923076923350, 1.000000000000000000 ),
 .UNSPECIFIED. ) 
 CURVE ( )  GEOMETRIC_REPRESENTATION_ITEM ( )  RATIONAL_B_SPLINE_CURVE ( ( 0.9786254102152882606, 0.9668223575118739532, 1.000000000000000000, 0.9510565162951535312, 1.000000000000000000, 0.9510565162951535312, 1.000000000000000000, 0.9510565162951535312, 1.000000000000000000, 0.9510565162951535312, 1.000000000000000000, 0.9510565162951535312, 1.000000000000000000, 0.9510565162951535312, 1.000000000000000000, 0.9510565162951535312, 1.000000000000000000, 0.9510565162951535312, 1.000000000000000000, 0.9510565162951535312, 1.000000000000000000, 0.9510565162951535312, 1.000000000000000000, 0.9510565162951535312, 1.000000000000000000, 0.9510565162951535312, 1.000000000000000000, 0.9510565162951535312, 1.000000000000000000, 0.9510565162951535312, 1.000000000000000000, 0.9510565162951535312, 1.000000000000000000, 0.9510565162951535312, 1.000000000000000000, 0.9510565162951535312, 1.000000000000000000, 0.9510565162951535312, 1.000000000000000000, 0.9510565162951535312, 1.000000000000000000, 0.9510565162951535312, 1.000000000000000000, 0.9510565162951535312, 1.000000000000000000, 0.9510565162951535312, 1.000000000000000000, 0.9510565162951535312, 1.000000000000000000, 0.9510565162951535312, 1.000000000000000000, 0.9510565162951535312, 1.000000000000000000, 0.9510565162951535312, 1.000000000000000000, 0.9510565162951535312, 1.000000000000000000, 0.9510565162951535312, 1.000000000000000000, 0.9510565162951535312, 1.000000000000000000, 0.9510565162951535312, 1.000000000000000000, 0.9510565162951535312, 1.000000000000000000, 0.9510565162951535312, 1.000000000000000000, 0.9510565162951535312, 1.000000000000000000, 0.9510565162951535312, 1.000000000000000000, 0.9510565162951535312, 1.000000000000000000, 0.9510565162951535312, 1.000000000000000000, 0.9510565162951535312, 1.000000000000000000, 0.9510565162951535312, 1.000000000000000000, 0.9510565162951535312, 1.000000000000000000, 0.9510565162951535312, 1.000000000000000000, 0.9510565162951535312, 1.000000000000000000, 0.9510565162951535312, 1.000000000000000000, 0.9510565162951535312, 1.000000000000000000, 0.9510565162951535312, 1.000000000000000000, 0.9510565162951535312, 1.000000000000000000, 0.9510565162951535312, 1.000000000000000000, 0.9510565162951535312, 1.000000000000000000, 0.9510565162951535312, 1.000000000000000000, 0.9510565162951535312, 1.000000000000000000, 0.9510565162951535312, 1.000000000000000000, 0.9510565162951535312, 1.000000000000000000, 0.9510565162951535312, 1.000000000000000000, 0.9510565162951535312, 1.000000000000000000, 0.9510565162951535312, 1.000000000000000000, 0.9510565162951535312, 1.000000000000000000, 0.9510565162951535312, 1.000000000000000000, 0.9510565162951535312, 1.000000000000000000, 0.9510565162951535312, 1.000000000000000000, 0.9510565162951535312, 1.000000000000000000, 0.9510565162951535312, 1.000000000000000000, 0.9510565162951535312, 1.000000000000000000, 0.9510565162951535312, 1.000000000000000000, 0.9510565162951535312, 1.000000000000000000, 0.9510565162951535312, 1.000000000000000000, 0.9510565162951535312, 1.000000000000000000, 0.9510565162951535312, 1.000000000000000000, 0.9510565162951535312, 1.000000000000000000, 0.9510565162951535312, 1.000000000000000000, 0.9510565162951535312, 1.000000000000000000, 0.9510565162951535312, 1.000000000000000000, 0.9510565162951535312, 1.000000000000000000, 0.9510565162951535312, 1.000000000000000000, 0.9510565162951535312, 1.000000000000000000, 0.9510565162951535312, 1.000000000000000000, 0.9510565162951535312, 1.000000000000000000, 0.9510565162951535312, 1.000000000000000000, 0.9510565162951535312, 1.000000000000000000, 0.9510565162951535312, 1.000000000000000000, 0.9510565162951535312, 1.000000000000000000, 0.9510565162951535312, 1.000000000000000000, 0.9510565162951535312, 1.000000000000000000, 0.9510565162951535312, 1.000000000000000000, 0.9510565162951535312, 1.000000000000000000, 0.9510565162951535312, 1.000000000000000000, 0.9510565162951535312, 1.000000000000000000, 0.9510565162951535312, 1.000000000000000000, 0.9510565162951535312, 1.000000000000000000, 0.9510565162951535312, 1.000000000000000000, 0.9510565162951535312, 1.000000000000000000, 0.9510565162951535312, 1.000000000000000000, 0.9510565162951535312, 1.000000000000000000, 0.9510565162951535312, 1.000000000000000000, 0.9510565162951535312, 1.000000000000000000, 0.9510565162951535312, 1.000000000000000000, 0.9510565162951535312, 1.000000000000000000, 0.9510565162951535312, 1.000000000000000000, 0.9510565162951535312, 1.000000000000000000, 0.9510565162951535312, 1.000000000000000000, 0.9510565162951535312, 1.000000000000000000, 0.9510565162951535312, 1.000000000000000000, 0.9510565162951535312, 1.000000000000000000, 0.9510565162951535312, 1.000000000000000000, 0.9510565162951535312, 1.000000000000000000, 0.9510565162951535312, 1.000000000000000000, 0.9510565162951535312, 1.000000000000000000, 0.9510565162951535312, 1.000000000000000000, 0.9510565162951535312, 1.000000000000000000, 0.9510565162951535312, 1.000000000000000000, 0.9510565162951535312, 1.000000000000000000, 0.9510565162951535312, 1.000000000000000000, 0.9510565162951535312, 1.000000000000000000, 0.9510565162951535312, 1.000000000000000000, 0.9510565162951535312, 1.000000000000000000, 0.9510565162951535312, 1.000000000000000000, 0.9510565162951535312, 1.000000000000000000, 0.9510565162951535312, 1.000000000000000000, 0.9510565162951535312, 1.000000000000000000, 0.9510565162951535312, 1.000000000000000000, 0.9510565162951535312, 1.000000000000000000, 0.9510565162951535312, 1.000000000000000000, 0.9510565162951535312, 1.000000000000000000, 0.9510565162951535312, 1.000000000000000000, 0.9510565162951535312, 1.000000000000000000, 0.9510565162951535312, 1.000000000000000000, 0.9510565162951535312, 1.000000000000000000, 0.9510565162951535312, 1.000000000000000000 ) ) 
 REPRESENTATION_ITEM ( '' )  );
#798 = AXIS2_PLACEMENT_3D ( 'NONE', #4981, #6292, #1833 ) ;
#799 = CARTESIAN_POINT ( 'NONE',  ( 4.784657899331211439, -89.10452850542925773, 1.454677039711774533 ) ) ;
#800 = CARTESIAN_POINT ( 'NONE',  ( 1.499999999999999556, -9.999999999999994671, -30.00000000000000000 ) ) ;
#801 = CARTESIAN_POINT ( 'NONE',  ( -2.369498399071204631, -93.15452850542925489, -6.969112962950009482 ) ) ;
#802 = VECTOR ( 'NONE', #5944, 1000.000000000000000 ) ;
#803 = CARTESIAN_POINT ( 'NONE',  ( 2.882544866740894829, -62.10452850542925063, 0.8366430509618999478 ) ) ;
#804 = DIRECTION ( 'NONE',  ( -1.000000000000000000, 0.000000000000000000, 0.000000000000000000 ) ) ;
#805 = CIRCLE ( 'NONE', #4298, 3.000000000000000000 ) ;
#806 = EDGE_CURVE ( 'NONE', #6097, #3730, #5164, .T. ) ;
#807 = LINE ( 'NONE', #39, #6725 ) ;
#808 = CARTESIAN_POINT ( 'NONE',  ( 1.840261337453270807, -76.80452850542926058, 2.371175808195547852 ) ) ;
#809 = CARTESIAN_POINT ( 'NONE',  ( -6.686770931921503625, -87.60452850542924352, -2.072711028461647675 ) ) ;
#810 = CARTESIAN_POINT ( 'NONE',  ( 50.00000000000000000, -19.99999999999999645, -12.50000000000000355 ) ) ;
#811 = CARTESIAN_POINT ( 'NONE',  ( -5.895805022753476621, -92.44547149457073942, -4.407101234057782868 ) ) ;
#812 = CARTESIAN_POINT ( 'NONE',  ( 47.50000000000002132, -51.00000000000000711, 12.50000000000001954 ) ) ;
#813 = DIRECTION ( 'NONE',  ( -0.000000000000000000, 0.000000000000000000, 1.000000000000000000 ) ) ;
#814 = CARTESIAN_POINT ( 'NONE',  ( -2.493201789345292241, -68.44547149457073942, -1.934965279058240561 ) ) ;
#815 =( NAMED_UNIT ( * ) PLANE_ANGLE_UNIT ( ) SI_UNIT ( $, .RADIAN. ) );
#816 = EDGE_LOOP ( 'NONE', ( #5885, #8217, #3994, #3810 ) ) ;
#817 = CARTESIAN_POINT ( 'NONE',  ( 4.784657899331208775, -68.10452850542925773, 1.454677039711774533 ) ) ;
#818 = CARTESIAN_POINT ( 'NONE',  ( -2.179377348189610153, -83.14547149457072805, -7.030887037049939003 ) ) ;
#819 = ORIENTED_EDGE ( 'NONE', *, *, #3574, .T. ) ;
#820 = CARTESIAN_POINT ( 'NONE',  ( -4.312004677471057867, -78.45452850542925205, -3.009306630940844052 ) ) ;
#821 = DIRECTION ( 'NONE',  ( 1.000000000000000000, -0.000000000000000000, -0.000000000000000000 ) ) ;
#822 = CARTESIAN_POINT ( 'NONE',  ( -3.015831842038130262, -66.19547149457075363, 3.989209796945492048 ) ) ;
#823 = CARTESIAN_POINT ( 'NONE',  ( 6.123233995736760366E-16, -27.00000000000000000, 5.000000000000000000 ) ) ;
#824 = CARTESIAN_POINT ( 'NONE',  ( -0.09506052544075783983, -66.49547149457075079, 2.999999999999997780 ) ) ;
#825 = CARTESIAN_POINT ( 'NONE',  ( -2.179377348189462271, -67.35452850542924352, 7.030887037049988741 ) ) ;
#826 = CARTESIAN_POINT ( 'NONE',  ( 80.00000000000000000, -25.00000000000000000, 20.00000000000000000 ) ) ;
#827 =( REPRESENTATION_RELATIONSHIP ('NONE','NONE', #4188, #1019 ) REPRESENTATION_RELATIONSHIP_WITH_TRANSFORMATION ( #2595 )SHAPE_REPRESENTATION_RELATIONSHIP( ) );
#828 = CARTESIAN_POINT ( 'NONE',  ( 80.00000000000000000, 2.168404344971008868E-15, -12.50000000000000000 ) ) ;
#829 = CARTESIAN_POINT ( 'NONE',  ( 4.312004677471078296, -88.95452850542922363, 3.009306630940844496 ) ) ;
#830 = CARTESIAN_POINT ( 'NONE',  ( 6.686770931921523164, -65.10452850542924352, 2.072711028461649008 ) ) ;
#831 = CARTESIAN_POINT ( 'NONE',  ( 2.823794231030060331, -79.09547149457075932, 1.017458915287723809 ) ) ;
#832 = ORIENTED_EDGE ( 'NONE', *, *, #1520, .T. ) ;
#833 = CARTESIAN_POINT ( 'NONE',  ( 54.99999999999999289, 80.00000000000000000, -7.500000000000000000 ) ) ;
#834 = CARTESIAN_POINT ( 'NONE',  ( 1.529537955723692999, -95.85452850542922931, -5.030887037049978971 ) ) ;
#835 = CARTESIAN_POINT ( 'NONE',  ( 0.09506052544086197875, -91.50452850542924921, 4.999999999999997335 ) ) ;
#836 = EDGE_LOOP ( 'NONE', ( #887, #6399, #4325, #7473 ) ) ;
#837 = CARTESIAN_POINT ( 'NONE',  ( -5.257311121191325043, -72.75452850542924921, 0.09995255151729529053 ) ) ;
#838 = CARTESIAN_POINT ( 'NONE',  ( 0.8796985632579634729, -90.64547149457075648, 3.030887037049952326 ) ) ;
#839 = CARTESIAN_POINT ( 'NONE',  ( -4.194503406049316041, -85.05452850542926058, 3.171033256558100533 ) ) ;
#840 = CARTESIAN_POINT ( 'NONE',  ( -4.037591185471547384, -59.29547149457074084, -5.718994135553860936 ) ) ;
#841 = CARTESIAN_POINT ( 'NONE',  ( 0.09506052544083729017, -64.50452850542926342, 2.999999999999997780 ) ) ;
#842 = EDGE_CURVE ( 'NONE', #7792, #3832, #1325, .T. ) ;
#843 = EDGE_CURVE ( 'NONE', #7540, #3412, #107, .T. ) ;
#844 = CARTESIAN_POINT ( 'NONE',  ( 1.499999999999999556, -9.999999999999994671, 0.000000000000000000 ) ) ;
#845 = FACE_OUTER_BOUND ( 'NONE', #4405, .T. ) ;
#846 = CARTESIAN_POINT ( 'NONE',  ( 1.686450176301585335, -74.70452850542925205, -2.482926158054133303 ) ) ;
#847 = CARTESIAN_POINT ( 'NONE',  ( -4.037591185471421262, -88.20452850542925205, 5.718994135553947977 ) ) ;
#848 = CARTESIAN_POINT ( 'NONE',  ( -4.037591185471543831, -86.29547149457074795, -5.718994135553860936 ) ) ;
#849 = PLANE ( 'NONE',  #2666 ) ;
#850 = CARTESIAN_POINT ( 'NONE',  ( 4.000000000000012434, -97.00000000000000000, 0.000000000000000000 ) ) ;
#851 = CARTESIAN_POINT ( 'NONE',  ( 3.154386672714807105, -64.24547149457075079, 0.09995255151720662534 ) ) ;
#852 = CYLINDRICAL_SURFACE ( 'NONE', #6905, 1.500000000000000666 ) ;
#853 = AXIS2_PLACEMENT_3D ( 'NONE', #1845, #3229, #5871 ) ;
#854 = EDGE_LOOP ( 'NONE', ( #4741, #415 ) ) ;
#855 = CARTESIAN_POINT ( 'NONE',  ( 4.725907263620340082, -68.40452850542925489, -1.635492904037697981 ) ) ;
#856 = CARTESIAN_POINT ( 'NONE',  ( -2.369498399071056305, -81.34547149457074511, 6.969112962950058332 ) ) ;
#857 = SHAPE_REPRESENTATION_RELATIONSHIP ( 'NONE' , 'NONE' ,  #1989, #7100 ) ;
#858 = ORIENTED_EDGE ( 'NONE', *, *, #2230, .T. ) ;
#859 = CARTESIAN_POINT ( 'NONE',  ( -2.862020680886495416, -67.20452850542925205, 4.100960146804039752 ) ) ;
#860 = AXIS2_PLACEMENT_3D ( 'NONE', #117, #1429, #3374 ) ;
#861 = CARTESIAN_POINT ( 'NONE',  ( 80.00000000000000000, 0.000000000000000000, 20.00000000000000000 ) ) ;
#862 = VECTOR ( 'NONE', #1618, 1000.000000000000227 ) ;
#863 = ITEM_DEFINED_TRANSFORMATION ( 'NONE', 'NONE', #5768,  #2840 ) ;
#864 = VECTOR ( 'NONE', #7310, 1000.000000000000000 ) ;
#865 = CARTESIAN_POINT ( 'NONE',  ( 5.257311121191341918, -70.24547149457075079, 0.09995255151718437925 ) ) ;
#866 = EDGE_CURVE ( 'NONE', #5004, #3412, #7048, .T. ) ;
#867 = DIRECTION ( 'NONE',  ( 0.000000000000000000, -1.000000000000000000, 3.469446951953615175E-16 ) ) ;
#868 = CARTESIAN_POINT ( 'NONE',  ( 2.610703060766943029, -61.54547149457074084, -1.773238653441125523 ) ) ;
#869 = CARTESIAN_POINT ( 'NONE',  ( -6.628020296210623385, -60.90452850542925489, 2.253526892787613978 ) ) ;
#870 = EDGE_LOOP ( 'NONE', ( #2926, #8293, #8072, #1678, #8003 ) ) ;
#871 = CARTESIAN_POINT ( 'NONE',  ( 50.00000000000000000, -9.999999999999992895, 4.499999999999999112 ) ) ;
#872 = CARTESIAN_POINT ( 'NONE',  ( 1.719659006605392060, -85.65452850542922647, 4.969112962950016588 ) ) ;
#873 = CARTESIAN_POINT ( 'NONE',  ( -6.686770931921507177, -63.60452850542924352, -2.072711028461647675 ) ) ;
#874 = CARTESIAN_POINT ( 'NONE',  ( 3.154386672714809325, -76.24547149457073658, 0.09995255151720662534 ) ) ;
#875 = EDGE_LOOP ( 'NONE', ( #4314, #1494, #2609, #7246 ) ) ;
#876 = CARTESIAN_POINT ( 'NONE',  ( 50.00000000000000000, -12.00000000000000355, -12.50000000000000178 ) ) ;
#877 = CARTESIAN_POINT ( 'NONE',  ( 0.000000000000000000, -9.999999999999994671, 0.000000000000000000 ) ) ;
#878 = CARTESIAN_POINT ( 'NONE',  ( 3.015831842038234178, -79.80452850542926058, 3.989209796945429432 ) ) ;
#879 = ADVANCED_FACE ( 'NONE', ( #1961 ), #7726, .F. ) ;
#880 = ORIENTED_EDGE ( 'NONE', *, *, #6640, .T. ) ;
#881 = CARTESIAN_POINT ( 'NONE',  ( 3.015831842038233734, -73.80452850542926058, 3.989209796945429432 ) ) ;
#882 = CARTESIAN_POINT ( 'NONE',  ( -2.823794231030039015, -86.59547149457075932, -1.017458915287723364 ) ) ;
#883 = APPLICATION_CONTEXT ( 'automotive_design' ) ;
#884 = CARTESIAN_POINT ( 'NONE',  ( 1.529537955723798026, -96.64547149457071384, 5.030887037049945221 ) ) ;
#885 = CARTESIAN_POINT ( 'NONE',  ( -0.09506052544085913381, -93.00452850542926342, -6.999999999999997335 ) ) ;
#886 = CARTESIAN_POINT ( 'NONE',  ( -3.154386672714790674, -69.75452850542926342, 0.09995255151727280851 ) ) ;
#887 = ORIENTED_EDGE ( 'NONE', *, *, #186, .T. ) ;
#888 = FACE_OUTER_BOUND ( 'NONE', #2508, .T. ) ;
#889 = FACE_BOUND ( 'NONE', #8067, .T. ) ;
#890 = CARTESIAN_POINT ( 'NONE',  ( 3.154386672714809325, -77.25452850542924921, -0.09995255151727241993 ) ) ;
#891 = CARTESIAN_POINT ( 'NONE',  ( 6.628020296210642037, -89.40452850542926910, -2.253526892787612645 ) ) ;
#892 = CARTESIAN_POINT ( 'NONE',  ( -2.369498399071055417, -90.34547149457073090, 6.969112962950058332 ) ) ;
#893 = CARTESIAN_POINT ( 'NONE',  ( 50.00000000000000000, -9.999999999999994671, 10.50000000000000533 ) ) ;
#894 = LINE ( 'NONE', #136, #4759 ) ;
#895 = CARTESIAN_POINT ( 'NONE',  ( -0.8796985632579434888, -71.14547149457074227, -3.030887037049952326 ) ) ;
#896 = UNCERTAINTY_MEASURE_WITH_UNIT (LENGTH_MEASURE( 1.000000000000000082E-05 ), #4515, 'distance_accuracy_value', 'NONE');
#897 = SURFACE_STYLE_USAGE ( .BOTH. , #2921 ) ;
#898 = ADVANCED_FACE ( 'NONE', ( #1362 ), #3345, .T. ) ;
#899 = ORIENTED_EDGE ( 'NONE', *, *, #2957, .F. ) ;
#900 = CARTESIAN_POINT ( 'NONE',  ( 4.312004677471073855, -64.95452850542926626, 3.009306630940844496 ) ) ;
#901 = CARTESIAN_POINT ( 'NONE',  ( -7.360235569667858968, -80.74547149457075079, -0.09995255151716124498 ) ) ;
#902 =( LENGTH_UNIT ( ) NAMED_UNIT ( * ) SI_UNIT ( .MILLI., .METRE. ) );
#903 = EDGE_CURVE ( 'NONE', #1902, #2390, #2584, .T. ) ;
#904 = EDGE_LOOP ( 'NONE', ( #7202, #2274, #7512, #7032, #7609 ) ) ;
#905 = CARTESIAN_POINT ( 'NONE',  ( -4.725907263620322318, -69.90452850542925489, 1.635492904037698647 ) ) ;
#906 = PLANE ( 'NONE',  #6654 ) ;
#907 = CARTESIAN_POINT ( 'NONE',  ( 2.862020680886598445, -66.79547149457073374, 4.100960146803977580 ) ) ;
#908 = CARTESIAN_POINT ( 'NONE',  ( 75.00000000000000000, 80.00000000000000000, 7.500000000000000000 ) ) ;
#909 = CARTESIAN_POINT ( 'NONE',  ( 4.312004677471013459, -94.54547149457071953, -3.009306630940933314 ) ) ;
#910 = CARTESIAN_POINT ( 'NONE',  ( -2.369498399071207739, -63.15452850542925489, -6.969112962950009482 ) ) ;
#911 = ORIENTED_EDGE ( 'NONE', *, *, #7757, .T. ) ;
#912 = DIRECTION ( 'NONE',  ( 0.8660254037844380415, 0.5000000000000011102, -0.000000000000000000 ) ) ;
#913 = CARTESIAN_POINT ( 'NONE',  ( 5.257311121191341918, -80.25452850542922079, -0.09995255151729465215 ) ) ;
#914 = VERTEX_POINT ( 'NONE', #3261 ) ;
#915 = DIRECTION ( 'NONE',  ( 0.000000000000000000, 1.000000000000000000, 2.775557561562891351E-16 ) ) ;
#916 = CARTESIAN_POINT ( 'NONE',  ( 4.725907263620341858, -86.40452850542926910, -1.635492904037697981 ) ) ;
#917 = CARTESIAN_POINT ( 'NONE',  ( 2.862020680886514512, -77.70452850542926626, -4.100960146804039752 ) ) ;
#918 = ORIENTED_EDGE ( 'NONE', *, *, #4017, .T. ) ;
#919 = CARTESIAN_POINT ( 'NONE',  ( -4.194503406049319594, -70.05452850542924637, 3.171033256558101865 ) ) ;
#920 = CARTESIAN_POINT ( 'NONE',  ( -1.840261337453198864, -87.19547149457073942, 2.371175808195584267 ) ) ;
#921 = CARTESIAN_POINT ( 'NONE',  ( -2.610703060766927930, -63.04547149457074084, 1.773238653441125745 ) ) ;
#922 = CARTESIAN_POINT ( 'NONE',  ( -4.784657899331190123, -78.60452850542925773, -1.454677039711773867 ) ) ;
#923 = CARTESIAN_POINT ( 'NONE',  ( -5.895805022753383362, -91.05452850542926058, 4.407101234057909878 ) ) ;
#924 = CARTESIAN_POINT ( 'NONE',  ( 2.882544866740894385, -59.10452850542926484, 0.8366430509618999478 ) ) ;
#925 = ORIENTED_EDGE ( 'NONE', *, *, #4635, .T. ) ;
#926 = DIRECTION ( 'NONE',  ( -0.000000000000000000, 0.000000000000000000, -1.000000000000000000 ) ) ;
#927 = ORIENTED_EDGE ( 'NONE', *, *, #4641, .T. ) ;
#928 = CARTESIAN_POINT ( 'NONE',  ( 6.000000000000004441, -27.99999999999999645, 2.500000000000000888 ) ) ;
#929 = CARTESIAN_POINT ( 'NONE',  ( 2.823794231030039903, -74.40452850542925489, -1.017458915287783316 ) ) ;
#930 = CARTESIAN_POINT ( 'NONE',  ( 4.037591185471444355, -89.70452850542925205, -5.718994135553947977 ) ) ;
#931 = EDGE_CURVE ( 'NONE', #6079, #3352, #634, .T. ) ;
#932 = VECTOR ( 'NONE', #2119, 1000.000000000000000 ) ;
#933 = CARTESIAN_POINT ( 'NONE',  ( 6.013306294175080779, -82.54547149457074795, -4.245374608440741326 ) ) ;
#934 = FACE_OUTER_BOUND ( 'NONE', #4950, .T. ) ;
#935 = DIRECTION ( 'NONE',  ( 0.000000000000000000, -1.000000000000000000, 0.000000000000000000 ) ) ;
#936 = CARTESIAN_POINT ( 'NONE',  ( 0.8796985632579601422, -63.64547149457072805, 3.030887037049952326 ) ) ;
#937 = EDGE_CURVE ( 'NONE', #8122, #5636, #7138, .T. ) ;
#938 = CARTESIAN_POINT ( 'NONE',  ( 6.000000000000006217, -51.00000000000000711, 2.500000000000000888 ) ) ;
#939 = ORIENTED_EDGE ( 'NONE', *, *, #6746, .T. ) ;
#940 = CARTESIAN_POINT ( 'NONE',  ( 54.99999999999999289, 80.00000000000000000, -7.500000000000000000 ) ) ;
#941 = CARTESIAN_POINT ( 'NONE',  ( -4.194503406049320482, -64.05452850542926058, 3.171033256558100533 ) ) ;
#942 = CARTESIAN_POINT ( 'NONE',  ( 2.179377348189629693, -78.64547149457074227, 7.030887037049939003 ) ) ;
#943 = VERTEX_POINT ( 'NONE', #2633 ) ;
#944 = VECTOR ( 'NONE', #2202, 1000.000000000000000 ) ;
#945 = CARTESIAN_POINT ( 'NONE',  ( 4.312004677471011682, -79.54547149457074795, -3.009306630940932425 ) ) ;
#946 = CARTESIAN_POINT ( 'NONE',  ( -1.529537955723777598, -74.14547149457074227, -5.030887037049945221 ) ) ;
#947 = CARTESIAN_POINT ( 'NONE',  ( -4.725907263620322318, -66.90452850542925489, 1.635492904037698647 ) ) ;
#948 = DIRECTION ( 'NONE',  ( -1.000000000000000000, 0.000000000000000000, 0.000000000000000000 ) ) ;
#949 = MECHANICAL_DESIGN_GEOMETRIC_PRESENTATION_REPRESENTATION (  '', ( #1216 ), #1896 ) ;
#950 = ADVANCED_FACE ( 'NONE', ( #47 ), #7770, .T. ) ;
#951 = CARTESIAN_POINT ( 'NONE',  ( -3.015831842038129817, -72.19547149457073942, 3.989209796945492048 ) ) ;
#952 = PLANE ( 'NONE',  #4975 ) ;
#953 = CARTESIAN_POINT ( 'NONE',  ( -0.09506052544086292244, -63.00452850542925631, -6.999999999999997335 ) ) ;
#954 = ORIENTED_EDGE ( 'NONE', *, *, #8275, .F. ) ;
#955 = SURFACE_SIDE_STYLE ('',( #6681 ) ) ;
#956 = ORIENTED_EDGE ( 'NONE', *, *, #4149, .T. ) ;
#957 = PLANE ( 'NONE',  #3547 ) ;
#958 = CARTESIAN_POINT ( 'NONE',  ( 4.312004677471078296, -85.95452850542925205, 3.009306630940844496 ) ) ;
#959 = CARTESIAN_POINT ( 'NONE',  ( 4.725907263620340970, -80.40452850542925489, -1.635492904037697981 ) ) ;
#960 = ADVANCED_FACE ( 'NONE', ( #722, #3931 ), #2758, .F. ) ;
#961 = ORIENTED_EDGE ( 'NONE', *, *, #806, .T. ) ;
#962 = CARTESIAN_POINT ( 'NONE',  ( -4.312004677471058756, -69.45452850542925205, -3.009306630940843608 ) ) ;
#963 = CARTESIAN_POINT ( 'NONE',  ( 1.069819614139495112, -82.84547149457074511, -2.969112962950042789 ) ) ;
#964 = CARTESIAN_POINT ( 'NONE',  ( -1.840261337453202195, -63.19547149457074653, 2.371175808195584267 ) ) ;
#965 = CARTESIAN_POINT ( 'NONE',  ( -4.312004677471057867, -75.45452850542925205, -3.009306630940844052 ) ) ;
#966 = CARTESIAN_POINT ( 'NONE',  ( 6.686770931921525829, -86.10452850542924352, 2.072711028461649008 ) ) ;
#967 = CARTESIAN_POINT ( 'NONE',  ( 1.840261337453222179, -94.69547149457076785, -2.371175808195584267 ) ) ;
#968 = EDGE_LOOP ( 'NONE', ( #6723, #4873, #5987, #7324 ) ) ;
#969 = CARTESIAN_POINT ( 'NONE',  ( -5.999999999999988454, -100.0010000000000048, -2.499999999999999112 ) ) ;
#970 = VERTEX_POINT ( 'NONE', #3218 ) ;
#971 = DIRECTION ( 'NONE',  ( -1.000000000000000000, 0.000000000000000000, 0.000000000000000000 ) ) ;
#972 = CARTESIAN_POINT ( 'NONE',  ( -2.493201789345253605, -64.05452850542924637, 1.934965279058294518 ) ) ;
#973 = CARTESIAN_POINT ( 'NONE',  ( -4.037591185471423039, -76.20452850542925205, 5.718994135553947977 ) ) ;
#974 = EDGE_CURVE ( 'NONE', #4167, #3662, #5, .T. ) ;
#975 = CARTESIAN_POINT ( 'NONE',  ( 6.686770931921479644, -82.39547149457074227, -2.072711028461788896 ) ) ;
#976 = CARTESIAN_POINT ( 'NONE',  ( -80.00000000000000000, -47.00000000000000711, -12.50000000000000888 ) ) ;
#977 = CARTESIAN_POINT ( 'NONE',  ( 3.015831842038151134, -94.69547149457075363, -3.989209796945492048 ) ) ;
#978 = CARTESIAN_POINT ( 'NONE',  ( 1.840261337453271473, -82.80452850542926058, 2.371175808195547852 ) ) ;
#979 = UNCERTAINTY_MEASURE_WITH_UNIT (LENGTH_MEASURE( 1.000000000000000082E-05 ), #1240, 'distance_accuracy_value', 'NONE');
#980 = CYLINDRICAL_SURFACE ( 'NONE', #1948, 1.499999999999994449 ) ;
#981 = VERTEX_POINT ( 'NONE', #4551 ) ;
#982 = LINE ( 'NONE', #2298, #7323 ) ;
#983 = CARTESIAN_POINT ( 'NONE',  ( -0.09506052544084110656, -69.00452850542926342, -4.999999999999997335 ) ) ;
#984 = CARTESIAN_POINT ( 'NONE',  ( -2.179377348189610597, -77.14547149457074227, -7.030887037049939003 ) ) ;
#985 = SURFACE_STYLE_USAGE ( .BOTH. , #1105 ) ;
#986 = ORIENTED_EDGE ( 'NONE', *, *, #669, .T. ) ;
#987 = CARTESIAN_POINT ( 'NONE',  ( 4.312004677471011682, -76.54547149457073374, -3.009306630940932425 ) ) ;
#988 = CARTESIAN_POINT ( 'NONE',  ( 4.312004677471011682, -70.54547149457074795, -3.009306630940933314 ) ) ;
#989 = CARTESIAN_POINT ( 'NONE',  ( 5.257311121191341918, -62.25452850542924921, -0.09995255151729465215 ) ) ;
#990 = DIRECTION ( 'NONE',  ( 0.5000000000000011102, -0.8660254037844380415, 0.000000000000000000 ) ) ;
#991 = EDGE_CURVE ( 'NONE', #2858, #7184, #5232, .T. ) ;
#992 = APPLICATION_CONTEXT ( 'automotive_design' ) ;
#993 = CARTESIAN_POINT ( 'NONE',  ( 3.015831842038147581, -67.69547149457073942, -3.989209796945492048 ) ) ;
#994 = VECTOR ( 'NONE', #495, 1000.000000000000000 ) ;
#995 = CARTESIAN_POINT ( 'NONE',  ( -4.191402346623181785, -57.30452850542924637, -5.607243785695311900 ) ) ;
#996 = VERTEX_POINT ( 'NONE', #2046 ) ;
#997 = CARTESIAN_POINT ( 'NONE',  ( 63.45299461620744808, 100.0000000000000000, 7.500000000000000000 ) ) ;
#998 = CIRCLE ( 'NONE', #3155, 1.500000000000001998 ) ;
#999 = ORIENTED_EDGE ( 'NONE', *, *, #7718, .T. ) ;
#1000 = DIRECTION ( 'NONE',  ( -0.000000000000000000, 1.000000000000000000, 2.775557561562891351E-16 ) ) ;
#1001 = CARTESIAN_POINT ( 'NONE',  ( 3.015831842038235511, -88.80452850542926058, 3.989209796945429432 ) ) ;
#1002 = CARTESIAN_POINT ( 'NONE',  ( -2.862020680886493640, -82.20452850542925205, 4.100960146804039752 ) ) ;
#1003 = ORIENTED_EDGE ( 'NONE', *, *, #842, .F. ) ;
#1004 = CARTESIAN_POINT ( 'NONE',  ( 4.312004677471076519, -73.95452850542926626, 3.009306630940844052 ) ) ;
#1005 = CARTESIAN_POINT ( 'NONE',  ( 0.09506052544077629729, -76.99547149457075079, -2.999999999999997780 ) ) ;
#1006 = VECTOR ( 'NONE', #1758, 1000.000000000000114 ) ;
#1007 = CARTESIAN_POINT ( 'NONE',  ( 1.719659006605287921, -97.84547149457071669, -4.969112962950050338 ) ) ;
#1008 = CARTESIAN_POINT ( 'NONE',  ( -4.784657899331191899, -63.60452850542925063, -1.454677039711773867 ) ) ;
#1009 = CARTESIAN_POINT ( 'NONE',  ( 6.686770931921525829, -89.10452850542925773, 2.072711028461649008 ) ) ;
#1010 = CARTESIAN_POINT ( 'NONE',  ( -1.840261337453253931, -60.30452850542926058, -2.371175808195547852 ) ) ;
#1011 = DIRECTION ( 'NONE',  ( 1.000000000000000000, 0.000000000000000000, 0.000000000000000000 ) ) ;
#1012 = VERTEX_POINT ( 'NONE', #135 ) ;
#1013 = DIRECTION ( 'NONE',  ( 0.000000000000000000, 0.7071067811865442421, -0.7071067811865509034 ) ) ;
#1014 = EDGE_LOOP ( 'NONE', ( #7055, #2724, #2403, #4042, #1733, #6191, #4300, #4661, #6588 ) ) ;
#1015 = CARTESIAN_POINT ( 'NONE',  ( 2.862020680886516732, -95.70452850542926626, -4.100960146804039752 ) ) ;
#1016 = CARTESIAN_POINT ( 'NONE',  ( 2.882544866740895717, -68.10452850542924352, 0.8366430509618999478 ) ) ;
#1017 = CARTESIAN_POINT ( 'NONE',  ( -6.686770931921458327, -83.89547149457074227, 2.072711028461789784 ) ) ;
#1018 = DIRECTION ( 'NONE',  ( 0.000000000000000000, -1.000000000000000000, -1.734723475976807094E-16 ) ) ;
#1019 = SHAPE_REPRESENTATION ( 'jaw', ( #2840 ), #1628 ) ;
#1020 = CARTESIAN_POINT ( 'NONE',  ( -4.784657899331156372, -92.89547149457075648, 1.454677039711874675 ) ) ;
#1021 = CARTESIAN_POINT ( 'NONE',  ( -2.882544866740875733, -87.60452850542924352, -0.8366430509618996147 ) ) ;
#1022 = DIRECTION ( 'NONE',  ( 0.000000000000000000, 0.000000000000000000, -1.000000000000000000 ) ) ;
#1023 = EDGE_LOOP ( 'NONE', ( #7409, #4492, #6931, #3372 ) ) ;
#1024 = CARTESIAN_POINT ( 'NONE',  ( 80.00000000000000000, 0.000000000000000000, -20.00000000000000000 ) ) ;
#1025 = CARTESIAN_POINT ( 'NONE',  ( 0.8796985632579013004, -95.85452850542924352, -3.030887037049972310 ) ) ;
#1026 = CARTESIAN_POINT ( 'NONE',  ( -7.360235569667858968, -74.74547149457073658, -0.09995255151716124498 ) ) ;
#1027 = CARTESIAN_POINT ( 'NONE',  ( -1.500000000000001110, -27.00000000000000000, 2.500000000000000888 ) ) ;
#1028 = CARTESIAN_POINT ( 'NONE',  ( -1.529537955723777154, -77.14547149457074227, -5.030887037049945221 ) ) ;
#1029 = CARTESIAN_POINT ( 'NONE',  ( 2.862020680886598445, -66.79547149457073374, 4.100960146803977580 ) ) ;
#1030 = CARTESIAN_POINT ( 'NONE',  ( 4.725907263620339194, -62.40452850542925489, -1.635492904037697981 ) ) ;
#1031 = CARTESIAN_POINT ( 'NONE',  ( 47.49999999999999289, -46.99999999999998579, 12.49999999999998224 ) ) ;
#1032 = ADVANCED_FACE ( 'NONE', ( #4469 ), #4594, .T. ) ;
#1033 = CARTESIAN_POINT ( 'NONE',  ( -4.194503406049384431, -65.44547149457072521, -3.171033256558012159 ) ) ;
#1034 =( LENGTH_UNIT ( ) NAMED_UNIT ( * ) SI_UNIT ( .MILLI., .METRE. ) );
#1035 = CARTESIAN_POINT ( 'NONE',  ( -5.895805022753386915, -64.05452850542924637, 4.407101234057909878 ) ) ;
#1036 = EDGE_LOOP ( 'NONE', ( #4830, #7266, #8107, #6146, #1939, #5954, #3636, #3435 ) ) ;
#1037 = ADVANCED_FACE ( 'NONE', ( #3889 ), #7135, .F. ) ;
#1038 = DIRECTION ( 'NONE',  ( -0.000000000000000000, 0.000000000000000000, 1.000000000000000000 ) ) ;
#1039 = PRODUCT_DEFINITION_SHAPE ( 'NONE', 'NONE',  #8343 ) ;
#1040 = EDGE_LOOP ( 'NONE', ( #1925, #1101, #1165, #6177 ) ) ;
#1041 = CARTESIAN_POINT ( 'NONE',  ( 1.223768561234547464E-14, -97.00000000000000000, 0.000000000000000000 ) ) ;
#1042 = CARTESIAN_POINT ( 'NONE',  ( -4.194503406049315153, -91.05452850542923215, 3.171033256558100533 ) ) ;
#1043 = CARTESIAN_POINT ( 'NONE',  ( 1.719659006605391616, -82.65452850542925489, 4.969112962950016588 ) ) ;
#1044 = CARTESIAN_POINT ( 'NONE',  ( 1.529537955723689002, -65.85452850542922931, -5.030887037049978971 ) ) ;
#1045 = CARTESIAN_POINT ( 'NONE',  ( 2.882544866740877509, -76.39547149457074227, -0.8366430509619593447 ) ) ;
#1046 = CARTESIAN_POINT ( 'NONE',  ( 4.194503406049402194, -93.94547149457075363, 3.171033256558012159 ) ) ;
#1047 = CARTESIAN_POINT ( 'NONE',  ( -5.257311121191324155, -69.75452850542926342, 0.09995255151729526277 ) ) ;
#1048 = CARTESIAN_POINT ( 'NONE',  ( -6.013306294175149169, -90.45452850542926626, -4.245374608440613429 ) ) ;
#1049 = MECHANICAL_DESIGN_GEOMETRIC_PRESENTATION_REPRESENTATION (  '', ( #4809 ), #4356 ) ;
#1050 = CARTESIAN_POINT ( 'NONE',  ( 2.493201789345311781, -93.94547149457073942, 1.934965279058241006 ) ) ;
#1051 = CONTEXT_DEPENDENT_SHAPE_REPRESENTATION ( #1698, #5477 ) ;
#1052 = EDGE_LOOP ( 'NONE', ( #3029, #343, #320, #925 ) ) ;
#1053 = DIRECTION ( 'NONE',  ( 0.000000000000000000, 0.000000000000000000, 1.000000000000000000 ) ) ;
#1054 = CARTESIAN_POINT ( 'NONE',  ( 2.862020680886516288, -92.70452850542926626, -4.100960146804039752 ) ) ;
#1055 = CARTESIAN_POINT ( 'NONE',  ( 2.823794231030039459, -68.40452850542925489, -1.017458915287783316 ) ) ;
#1056 = CARTESIAN_POINT ( 'NONE',  ( 4.191402346623079644, -82.69547149457073942, -5.607243785695398941 ) ) ;
#1057 = FACE_OUTER_BOUND ( 'NONE', #2231, .T. ) ;
#1058 = CARTESIAN_POINT ( 'NONE',  ( -5.257311121191321490, -95.74547149457072237, -0.09995255151718372699 ) ) ;
#1059 = CARTESIAN_POINT ( 'NONE',  ( 0.09506052544083956612, -82.50452850542926342, 2.999999999999997780 ) ) ;
#1060 = EDGE_CURVE ( 'NONE', #6118, #5503, #2083, .T. ) ;
#1061 = CARTESIAN_POINT ( 'NONE',  ( 75.00000000000000000, 80.00000000000000000, 7.500000000000000000 ) ) ;
#1062 = EDGE_LOOP ( 'NONE', ( #5478, #3548, #403, #6706 ) ) ;
#1063 = CYLINDRICAL_SURFACE ( 'NONE', #189, 1.500000000000000666 ) ;
#1064 = CARTESIAN_POINT ( 'NONE',  ( -2.493201789345250052, -94.05452850542926058, 1.934965279058294518 ) ) ;
#1065 = CARTESIAN_POINT ( 'NONE',  ( 6.013306294175077227, -70.54547149457074795, -4.245374608440741326 ) ) ;
#1066 = SHAPE_REPRESENTATION ( 'return spring', ( #2840 ), #3385 ) ;
#1067 = CARTESIAN_POINT ( 'NONE',  ( 3.783624887602714981, -96.99999999999998579, -4.615931839566195904 ) ) ;
#1068 = CARTESIAN_POINT ( 'NONE',  ( -2.862020680886581125, -71.29547149457074795, -4.100960146803977580 ) ) ;
#1069 = CARTESIAN_POINT ( 'NONE',  ( 4.194503406049400418, -66.94547149457075363, 3.171033256558012159 ) ) ;
#1070 = CARTESIAN_POINT ( 'NONE',  ( 4.312004677471073855, -58.95452850542925205, 3.009306630940844496 ) ) ;
#1071 = DIRECTION ( 'NONE',  ( -9.251858538542971581E-17, 1.000000000000000000, -0.000000000000000000 ) ) ;
#1072 = MECHANICAL_DESIGN_GEOMETRIC_PRESENTATION_REPRESENTATION (  '', ( #7261 ), #2289 ) ;
#1073 = VECTOR ( 'NONE', #4781, 1000.000000000000000 ) ;
#1074 = CARTESIAN_POINT ( 'NONE',  ( 7.360235569667880284, -97.24547149457075079, 0.09995255151716216091 ) ) ;
#1075 = CARTESIAN_POINT ( 'NONE',  ( -3.015831842038213306, -93.30452850542926058, -3.989209796945429432 ) ) ;
#1076 = ORIENTED_EDGE ( 'NONE', *, *, #1253, .F. ) ;
#1077 = UNCERTAINTY_MEASURE_WITH_UNIT (LENGTH_MEASURE( 1.000000000000000082E-05 ), #5419, 'distance_accuracy_value', 'NONE');
#1078 = CARTESIAN_POINT ( 'NONE',  ( 6.123233995736760366E-16, -27.00000000000000000, 4.500000000000000888 ) ) ;
#1079 = MECHANICAL_DESIGN_GEOMETRIC_PRESENTATION_REPRESENTATION (  '', ( #5919 ), #7416 ) ;
#1080 = ORIENTED_EDGE ( 'NONE', *, *, #5142, .T. ) ;
#1081 = LINE ( 'NONE', #4358, #6236 ) ;
#1082 = CARTESIAN_POINT ( 'NONE',  ( 1.719659006605392060, -85.65452850542922647, 4.969112962950016588 ) ) ;
#1083 = CARTESIAN_POINT ( 'NONE',  ( -4.784657899331156372, -89.89547149457075648, 1.454677039711874675 ) ) ;
#1084 = CARTESIAN_POINT ( 'NONE',  ( 1.529537955723688780, -62.85452850542924352, -5.030887037049978971 ) ) ;
#1085 = CARTESIAN_POINT ( 'NONE',  ( -2.610703060766925265, -84.04547149457074795, 1.773238653441125745 ) ) ;
#1086 = CARTESIAN_POINT ( 'NONE',  ( -1.529537955723774711, -92.14547149457071384, -5.030887037049945221 ) ) ;
#1087 = CARTESIAN_POINT ( 'NONE',  ( 3.015831842038232846, -67.80452850542926058, 3.989209796945429432 ) ) ;
#1088 = CARTESIAN_POINT ( 'NONE',  ( -4.037591185471421262, -88.20452850542925205, 5.718994135553947977 ) ) ;
#1089 = CARTESIAN_POINT ( 'NONE',  ( 1.069819614139496666, -94.84547149457073090, -2.969112962950042789 ) ) ;
#1090 = ORIENTED_EDGE ( 'NONE', *, *, #3922, .T. ) ;
#1091 = DIRECTION ( 'NONE',  ( -0.000000000000000000, -0.000000000000000000, -1.000000000000000000 ) ) ;
#1092 = VERTEX_POINT ( 'NONE', #4012 ) ;
#1093 = CARTESIAN_POINT ( 'NONE',  ( 3.015831842038235955, -91.80452850542926058, 3.989209796945429432 ) ) ;
#1094 = CARTESIAN_POINT ( 'NONE',  ( 1.069819614139555730, -64.65452850542924068, 2.969112962950023249 ) ) ;
#1095 = CARTESIAN_POINT ( 'NONE',  ( 5.257311121191342806, -92.25452850542922079, -0.09995255151729465215 ) ) ;
#1096 = CARTESIAN_POINT ( 'NONE',  ( -7.360235569667858968, -74.74547149457073658, -0.09995255151716124498 ) ) ;
#1097 = CARTESIAN_POINT ( 'NONE',  ( -1.529537955723667908, -94.35452850542922931, 5.030887037049979860 ) ) ;
#1098 = EDGE_CURVE ( 'NONE', #2188, #4993, #6582, .T. ) ;
#1099 = CARTESIAN_POINT ( 'NONE',  ( 2.862020680886601998, -96.79547149457073374, 4.100960146803977580 ) ) ;
#1100 = CARTESIAN_POINT ( 'NONE',  ( -2.493201789345250940, -85.05452850542926058, 1.934965279058294518 ) ) ;
#1101 = ORIENTED_EDGE ( 'NONE', *, *, #5827, .T. ) ;
#1102 = FILL_AREA_STYLE ('',( #6916 ) ) ;
#1103 = CARTESIAN_POINT ( 'NONE',  ( 4.312004677471073855, -58.95452850542925205, 3.009306630940844496 ) ) ;
#1104 = CARTESIAN_POINT ( 'NONE',  ( 2.179377348189628361, -66.64547149457072805, 7.030887037049939003 ) ) ;
#1105 = SURFACE_SIDE_STYLE ('',( #1786 ) ) ;
#1106 = DIRECTION ( 'NONE',  ( -0.000000000000000000, -0.000000000000000000, -1.000000000000000000 ) ) ;
#1107 = PRODUCT_DEFINITION_SHAPE ( 'NONE', 'NONE',  #8340 ) ;
#1108 = CARTESIAN_POINT ( 'NONE',  ( -4.725907263620353405, -74.59547149457074511, -1.635492904037597617 ) ) ;
#1109 = CARTESIAN_POINT ( 'NONE',  ( -5.257311121191324155, -68.74547149457072237, -0.09995255151718371311 ) ) ;
#1110 = CARTESIAN_POINT ( 'NONE',  ( 1.529537955723688336, -59.85452850542924352, -5.030887037049978971 ) ) ;
#1111 = LINE ( 'NONE', #3683, #4625 ) ;
#1112 = VECTOR ( 'NONE', #3807, 1000.000000000000000 ) ;
#1113 = CARTESIAN_POINT ( 'NONE',  ( 4.784657899331208775, -68.10452850542925773, 1.454677039711774533 ) ) ;
#1114 = CARTESIAN_POINT ( 'NONE',  ( 4.312004677471010794, -61.54547149457073374, -3.009306630940933314 ) ) ;
#1115 = SURFACE_STYLE_FILL_AREA ( #8236 ) ;
#1116 = ORIENTED_EDGE ( 'NONE', *, *, #8084, .T. ) ;
#1117 = LINE ( 'NONE', #7526, #1006 ) ;
#1118 = ADVANCED_FACE ( 'NONE', ( #5950 ), #176, .F. ) ;
#1119 = ORIENTED_EDGE ( 'NONE', *, *, #4522, .F. ) ;
#1120 = LINE ( 'NONE', #1760, #8127 ) ;
#1121 = CARTESIAN_POINT ( 'NONE',  ( -1.719659006605371632, -81.15452850542922647, -4.969112962950016588 ) ) ;
#1122 = VECTOR ( 'NONE', #1414, 1000.000000000000000 ) ;
#1123 = CARTESIAN_POINT ( 'NONE',  ( 3.015831842038149802, -85.69547149457073942, -3.989209796945492048 ) ) ;
#1124 = CARTESIAN_POINT ( 'NONE',  ( 1.719659006605388507, -58.65452850542925489, 4.969112962950015699 ) ) ;
#1125 = CARTESIAN_POINT ( 'NONE',  ( 2.610703060766946138, -85.54547149457074795, -1.773238653441125523 ) ) ;
#1126 = CARTESIAN_POINT ( 'NONE',  ( -2.369498399071206407, -78.15452850542924068, -6.969112962950009482 ) ) ;
#1127 = CARTESIAN_POINT ( 'NONE',  ( 3.015831842038150246, -88.69547149457073942, -3.989209796945492048 ) ) ;
#1128 = CARTESIAN_POINT ( 'NONE',  ( -2.862020680886495416, -70.20452850542925205, 4.100960146804039752 ) ) ;
#1129 = CARTESIAN_POINT ( 'NONE',  ( -4.037591185471423039, -76.20452850542925205, 5.718994135553947977 ) ) ;
#1130 = AXIS2_PLACEMENT_3D ( 'NONE', #6423, #2642, #3184 ) ;
#1131 = AXIS2_PLACEMENT_3D ( 'NONE', #7941, #259, #5193 ) ;
#1132 = VECTOR ( 'NONE', #7276, 1000.000000000000000 ) ;
#1133 = VECTOR ( 'NONE', #778, 1000.000000000000000 ) ;
#1134 = CARTESIAN_POINT ( 'NONE',  ( -2.882544866740855749, -92.89547149457074227, 0.8366430509619596778 ) ) ;
#1135 = PRODUCT_DEFINITION ( 'UNKNOWN', '', #8199, #8065 ) ;
#1136 = VERTEX_POINT ( 'NONE', #339 ) ;
#1137 = CARTESIAN_POINT ( 'NONE',  ( 45.96623493960122886, -14.74233734943963192, 4.500000000000000888 ) ) ;
#1138 = PRESENTATION_LAYER_ASSIGNMENT (  '', '', ( #8272 ) ) ;
#1139 = VERTEX_POINT ( 'NONE', #7940 ) ;
#1140 = CARTESIAN_POINT ( 'NONE',  ( -1.529537955723668130, -94.35452850542924352, 5.030887037049979860 ) ) ;
#1141 = CARTESIAN_POINT ( 'NONE',  ( 1.840261337453269919, -67.80452850542926058, 2.371175808195547852 ) ) ;
#1142 = CARTESIAN_POINT ( 'NONE',  ( -0.09506052544083808120, -93.00452850542926342, -4.999999999999997335 ) ) ;
#1143 = CARTESIAN_POINT ( 'NONE',  ( 2.369498399071077177, -73.84547149457073090, -6.969112962950057444 ) ) ;
#1144 = CARTESIAN_POINT ( 'NONE',  ( 5.257311121191342806, -92.25452850542922079, -0.09995255151729465215 ) ) ;
#1145 = CARTESIAN_POINT ( 'NONE',  ( 3.015831842038150246, -88.69547149457073942, -3.989209796945492048 ) ) ;
#1146 = CARTESIAN_POINT ( 'NONE',  ( 2.882544866740898382, -89.10452850542925773, 0.8366430509618999478 ) ) ;
#1147 = EDGE_LOOP ( 'NONE', ( #8081, #927 ) ) ;
#1148 = CLOSED_SHELL ( 'NONE', ( #543, #2137, #6595, #3524 ) ) ;
#1149 = PRESENTATION_STYLE_ASSIGNMENT (( #3841 ) ) ;
#1150 = CARTESIAN_POINT ( 'NONE',  ( -4.194503406049320482, -61.05452850542923926, 3.171033256558100533 ) ) ;
#1151 = CARTESIAN_POINT ( 'NONE',  ( -6.013306294175061240, -69.04547149457074795, 4.245374608440741326 ) ) ;
#1152 = SURFACE_SIDE_STYLE ('',( #2418 ) ) ;
#1153 =( REPRESENTATION_RELATIONSHIP ('NONE','NONE', #4188, #7093 ) REPRESENTATION_RELATIONSHIP_WITH_TRANSFORMATION ( #4436 )SHAPE_REPRESENTATION_RELATIONSHIP( ) );
#1154 = CARTESIAN_POINT ( 'NONE',  ( 4.597760815568308068, -96.99999999999982947, 2.447692062181759720 ) ) ;
#1155 = CARTESIAN_POINT ( 'NONE',  ( -1.719659006605267493, -63.34547149457074511, 4.969112962950051227 ) ) ;
#1156 = CARTESIAN_POINT ( 'NONE',  ( 7.360235569667880284, -94.24547149457075079, 0.09995255151716216091 ) ) ;
#1157 = CARTESIAN_POINT ( 'NONE',  ( -1.686450176301564019, -91.20452850542925205, 2.482926158054133303 ) ) ;
#1158 = PLANE ( 'NONE',  #2220 ) ;
#1159 = ADVANCED_FACE ( 'NONE', ( #6622 ), #6113, .F. ) ;
#1160 = CARTESIAN_POINT ( 'NONE',  ( 5.257311121191341918, -71.25452850542923500, -0.09995255151729465215 ) ) ;
#1161 = CARTESIAN_POINT ( 'NONE',  ( -0.09506052544071151578, -96.49547149457075079, 6.999999999999997335 ) ) ;
#1162 = VERTEX_POINT ( 'NONE', #216 ) ;
#1163 = DIRECTION ( 'NONE',  ( 0.000000000000000000, 2.775557561562891351E-16, -1.000000000000000000 ) ) ;
#1164 = ADVANCED_FACE ( 'NONE', ( #4096, #7258 ), #4133, .F. ) ;
#1165 = ORIENTED_EDGE ( 'NONE', *, *, #4237, .T. ) ;
#1166 = DIRECTION ( 'NONE',  ( 1.000000000000000000, -0.000000000000000000, -0.000000000000000000 ) ) ;
#1167 = CARTESIAN_POINT ( 'NONE',  ( -5.257311121191324155, -72.75452850542924921, 0.09995255151729526277 ) ) ;
#1168 = CARTESIAN_POINT ( 'NONE',  ( -4.784657899331157260, -86.89547149457074227, 1.454677039711874675 ) ) ;
#1169 = CARTESIAN_POINT ( 'NONE',  ( -2.862020680886496748, -58.20452850542925916, 4.100960146804039752 ) ) ;
#1170 = CARTESIAN_POINT ( 'NONE',  ( -0.8796985632579434888, -71.14547149457074227, -3.030887037049952326 ) ) ;
#1171 = CARTESIAN_POINT ( 'NONE',  ( 4.191402346623197772, -76.80452850542926058, 5.607243785695311900 ) ) ;
#1172 = CARTESIAN_POINT ( 'NONE',  ( -4.784657899331156372, -92.89547149457075648, 1.454677039711874675 ) ) ;
#1173 = CARTESIAN_POINT ( 'NONE',  ( -1.719659006605374074, -63.15452850542925489, -4.969112962950016588 ) ) ;
#1174 = CARTESIAN_POINT ( 'NONE',  ( 2.179377348189482699, -80.85452850542925773, -7.030887037049986077 ) ) ;
#1175 = CARTESIAN_POINT ( 'NONE',  ( 1.686450176301636850, -84.79547149457074795, 2.482926158054096000 ) ) ;
#1176 = ORIENTED_EDGE ( 'NONE', *, *, #6774, .T. ) ;
#1177 = LINE ( 'NONE', #1816, #2009 ) ;
#1178 = CARTESIAN_POINT ( 'NONE',  ( -4.312004677470996583, -60.04547149457074084, 3.009306630940933314 ) ) ;
#1179 = EDGE_LOOP ( 'NONE', ( #5757, #6068, #5152, #5321, #3694 ) ) ;
#1180 = CARTESIAN_POINT ( 'NONE',  ( -4.312004677471055203, -93.45452850542925205, -3.009306630940843608 ) ) ;
#1181 = CARTESIAN_POINT ( 'NONE',  ( -2.493201789345288688, -95.44547149457075363, -1.934965279058240561 ) ) ;
#1182 = VECTOR ( 'NONE', #6075, 1000.000000000000000 ) ;
#1183 = CARTESIAN_POINT ( 'NONE',  ( -6.013306294175153610, -60.45452850542925916, -4.245374608440613429 ) ) ;
#1184 = CARTESIAN_POINT ( 'NONE',  ( -5.895805022753479285, -68.44547149457073942, -4.407101234057782868 ) ) ;
#1185 = CARTESIAN_POINT ( 'NONE',  ( 4.725907263620373833, -85.09547149457074511, 1.635492904037598283 ) ) ;
#1186 = CARTESIAN_POINT ( 'NONE',  ( -2.882544866740877954, -72.60452850542924352, -0.8366430509618996147 ) ) ;
#1187 = PLANE ( 'NONE',  #5298 ) ;
#1188 = ORIENTED_EDGE ( 'NONE', *, *, #2399, .T. ) ;
#1189 = LINE ( 'NONE', #3759, #453 ) ;
#1190 = CARTESIAN_POINT ( 'NONE',  ( 4.194503406049334693, -62.55452850542925347, -3.171033256558100089 ) ) ;
#1191 = CARTESIAN_POINT ( 'NONE',  ( -4.037591185471545607, -68.29547149457073374, -5.718994135553860936 ) ) ;
#1192 = CARTESIAN_POINT ( 'NONE',  ( 50.00000000000000000, -12.00000000000000355, -12.50000000000000178 ) ) ;
#1193 = CARTESIAN_POINT ( 'NONE',  ( -1.529537955723777820, -68.14547149457074227, -5.030887037049945221 ) ) ;
#1194 = CARTESIAN_POINT ( 'NONE',  ( -4.191402346623055664, -96.19547149457075363, 5.607243785695398941 ) ) ;
#1195 = CARTESIAN_POINT ( 'NONE',  ( 3.154386672714811102, -95.25452850542926342, -0.09995255151727241993 ) ) ;
#1196 = DIRECTION ( 'NONE',  ( 9.251858538542971581E-17, -1.000000000000000000, 0.000000000000000000 ) ) ;
#1197 = VECTOR ( 'NONE', #5715, 1000.000000000000000 ) ;
#1198 = CARTESIAN_POINT ( 'NONE',  ( 1.529537955723689224, -71.85452850542925773, -5.030887037049978971 ) ) ;
#1199 = CARTESIAN_POINT ( 'NONE',  ( -6.686770931921456551, -95.89547149457075648, 2.072711028461789784 ) ) ;
#1200 = ORIENTED_EDGE ( 'NONE', *, *, #6332, .F. ) ;
#1201 = AXIS2_PLACEMENT_3D ( 'NONE', #8228, #666, #7120 ) ;
#1202 = VECTOR ( 'NONE', #84, 1000.000000000000000 ) ;
#1203 = CARTESIAN_POINT ( 'NONE',  ( 45.00000000000000000, -19.99999999999999645, -12.50000000000000355 ) ) ;
#1204 = ADVANCED_FACE ( 'NONE', ( #1486 ), #849, .T. ) ;
#1205 = PRODUCT_CONTEXT ( 'NONE', #5879, 'mechanical' ) ;
#1206 = VECTOR ( 'NONE', #2792, 1000.000000000000000 ) ;
#1207 = ORIENTED_EDGE ( 'NONE', *, *, #4767, .T. ) ;
#1208 = DIRECTION ( 'NONE',  ( 1.000000000000000000, 0.000000000000000000, -0.000000000000000000 ) ) ;
#1209 = CARTESIAN_POINT ( 'NONE',  ( 2.862020680886514956, -80.70452850542925205, -4.100960146804039752 ) ) ;
#1210 = CARTESIAN_POINT ( 'NONE',  ( -3.015831842038127597, -87.19547149457073942, 3.989209796945492048 ) ) ;
#1211 = CARTESIAN_POINT ( 'NONE',  ( -5.257311121191325931, -57.75452850542924921, 0.09995255151729529053 ) ) ;
#1212 = CARTESIAN_POINT ( 'NONE',  ( 3.154386672714808437, -70.24547149457075079, 0.09995255151720662534 ) ) ;
#1213 = CARTESIAN_POINT ( 'NONE',  ( 7.360235569667878508, -83.25452850542926342, -0.09995255151731691212 ) ) ;
#1214 = CARTESIAN_POINT ( 'NONE',  ( 1.529537955723796472, -87.64547149457071384, 5.030887037049945221 ) ) ;
#1215 = CARTESIAN_POINT ( 'NONE',  ( 3.015831842038231958, -61.80452850542926058, 3.989209796945429432 ) ) ;
#1216 = STYLED_ITEM ( 'NONE', ( #5735 ), #7608 ) ;
#1217 = CARTESIAN_POINT ( 'NONE',  ( 7.360235569667877620, -77.25452850542924921, -0.09995255151731691212 ) ) ;
#1218 = CARTESIAN_POINT ( 'NONE',  ( -2.493201789345289132, -92.44547149457073942, -1.934965279058240561 ) ) ;
#1219 = ORIENTED_EDGE ( 'NONE', *, *, #8239, .T. ) ;
#1220 = DIRECTION ( 'NONE',  ( 1.000000000000000000, -0.000000000000000000, -0.000000000000000000 ) ) ;
#1221 = CARTESIAN_POINT ( 'NONE',  ( 75.00000000000000000, -20.00000000000000000, 7.500000000000000000 ) ) ;
#1222 = EDGE_LOOP ( 'NONE', ( #5531, #221 ) ) ;
#1223 = CARTESIAN_POINT ( 'NONE',  ( 5.257311121191343695, -92.25452850542924921, -0.09995255151729466603 ) ) ;
#1224 = CARTESIAN_POINT ( 'NONE',  ( -0.09506052544082083111, -63.00452850542925631, -2.999999999999997780 ) ) ;
#1225 = CARTESIAN_POINT ( 'NONE',  ( 4.191402346623195996, -58.80452850542926058, 5.607243785695311900 ) ) ;
#1226 = CARTESIAN_POINT ( 'NONE',  ( 4.191402346623077868, -73.69547149457073942, -5.607243785695398941 ) ) ;
#1227 = CARTESIAN_POINT ( 'NONE',  ( -1.719659006605263940, -90.34547149457074511, 4.969112962950051227 ) ) ;
#1228 = CARTESIAN_POINT ( 'NONE',  ( -1.686450176301565351, -79.20452850542925205, 2.482926158054133303 ) ) ;
#1229 = EDGE_CURVE ( 'NONE', #4621, #6524, #2166, .T. ) ;
#1230 = CARTESIAN_POINT ( 'NONE',  ( -2.823794231030019475, -87.90452850542926910, 1.017458915287783316 ) ) ;
#1231 = CARTESIAN_POINT ( 'NONE',  ( 6.628020296210686446, -64.09547149457071669, 2.253526892787472757 ) ) ;
#1232 = DIRECTION ( 'NONE',  ( 0.000000000000000000, 0.000000000000000000, -1.000000000000000000 ) ) ;
#1233 = CARTESIAN_POINT ( 'NONE',  ( 1.529537955723794251, -63.64547149457074227, 5.030887037049945221 ) ) ;
#1234 = CARTESIAN_POINT ( 'NONE',  ( 4.784657899331175912, -61.39547149457074227, -1.454677039711874009 ) ) ;
#1235 = CARTESIAN_POINT ( 'NONE',  ( -0.8796985632578772085, -94.35452850542925773, 3.030887037049973198 ) ) ;
#1236 = DIRECTION ( 'NONE',  ( 1.000000000000000000, 0.000000000000000000, 0.000000000000000000 ) ) ;
#1237 = CARTESIAN_POINT ( 'NONE',  ( -4.784657899331190123, -72.60452850542925773, -1.454677039711773867 ) ) ;
#1238 = EDGE_CURVE ( 'NONE', #3733, #5980, #6033, .T. ) ;
#1239 = CARTESIAN_POINT ( 'NONE',  ( 0.09506052544073614885, -91.99547149457075079, -6.999999999999997335 ) ) ;
#1240 =( LENGTH_UNIT ( ) NAMED_UNIT ( * ) SI_UNIT ( .MILLI., .METRE. ) );
#1241 = VERTEX_POINT ( 'NONE', #8061 ) ;
#1242 = CARTESIAN_POINT ( 'NONE',  ( 43.45299461620743386, -9.999999999999994671, 1.500000000000000666 ) ) ;
#1243 = CONTEXT_DEPENDENT_SHAPE_REPRESENTATION ( #1153, #6754 ) ;
#1244 = ORIENTED_EDGE ( 'NONE', *, *, #6774, .F. ) ;
#1245 = CARTESIAN_POINT ( 'NONE',  ( -80.00000000000000000, -25.00000000000000000, 20.00000000000000000 ) ) ;
#1246 = CARTESIAN_POINT ( 'NONE',  ( -1.529537955723670128, -79.35452850542925773, 5.030887037049979860 ) ) ;
#1247 = CARTESIAN_POINT ( 'NONE',  ( 4.725907263620374721, -88.09547149457074511, 1.635492904037598283 ) ) ;
#1248 = FACE_OUTER_BOUND ( 'NONE', #1759, .T. ) ;
#1249 = CARTESIAN_POINT ( 'NONE',  ( -2.493201789345291353, -74.44547149457072521, -1.934965279058240561 ) ) ;
#1250 = CARTESIAN_POINT ( 'NONE',  ( 2.179377348189481811, -74.85452850542925773, -7.030887037049986077 ) ) ;
#1251 = CARTESIAN_POINT ( 'NONE',  ( 0.09506052544075639654, -85.99547149457075079, -4.999999999999997335 ) ) ;
#1252 = FACE_OUTER_BOUND ( 'NONE', #159, .T. ) ;
#1253 = EDGE_CURVE ( 'NONE', #7447, #5257, #4677, .T. ) ;
#1254 = CARTESIAN_POINT ( 'NONE',  ( -4.191402346623179120, -75.30452850542926058, -5.607243785695311900 ) ) ;
#1255 = CARTESIAN_POINT ( 'NONE',  ( -3.154386672714788453, -86.74547149457075079, -0.09995255151720625064 ) ) ;
#1256 = AXIS2_PLACEMENT_3D ( 'NONE', #1926, #3778, #2010 ) ;
#1257 = ORIENTED_EDGE ( 'NONE', *, *, #2308, .T. ) ;
#1258 = CARTESIAN_POINT ( 'NONE',  ( 75.00000000000000000, -30.00000000000000000, -7.500000000000007105 ) ) ;
#1259 = CARTESIAN_POINT ( 'NONE',  ( -1.719659006605267937, -60.34547149457073800, 4.969112962950051227 ) ) ;
#1260 = ORIENTED_EDGE ( 'NONE', *, *, #358, .T. ) ;
#1261 = CARTESIAN_POINT ( 'NONE',  ( 5.257311121191342806, -80.25452850542924921, -0.09995255151729466603 ) ) ;
#1262 = CARTESIAN_POINT ( 'NONE',  ( -0.09506052544082159439, -57.00452850542925631, -2.999999999999997780 ) ) ;
#1263 = CARTESIAN_POINT ( 'NONE',  ( 4.312004677471078296, -91.95452850542925205, 3.009306630940844496 ) ) ;
#1264 = VECTOR ( 'NONE', #28, 1000.000000000000000 ) ;
#1265 =( GEOMETRIC_REPRESENTATION_CONTEXT ( 3 ) GLOBAL_UNCERTAINTY_ASSIGNED_CONTEXT ( ( #3607 ) ) GLOBAL_UNIT_ASSIGNED_CONTEXT ( ( #7000, #468, #5646 ) ) REPRESENTATION_CONTEXT ( 'NONE', 'WORKASPACE' ) );
#1266 = CARTESIAN_POINT ( 'NONE',  ( -4.191402346623058328, -72.19547149457073942, 5.607243785695398941 ) ) ;
#1267 = CARTESIAN_POINT ( 'NONE',  ( 1.529537955723796916, -87.64547149457072805, 5.030887037049945221 ) ) ;
#1268 = CARTESIAN_POINT ( 'NONE',  ( -2.882544866740877509, -75.60452850542924352, -0.8366430509618996147 ) ) ;
#1269 = VECTOR ( 'NONE', #3226, 1000.000000000000000 ) ;
#1270 = B_SPLINE_CURVE_WITH_KNOTS ( 'NONE', 3,
 ( #1416, #1972, #4441, #7829, #2057, #6429, #3274, #6553, #7149, #2514, #6392, #5078, #3149, #3231, #16, #62, #608, #8285, #1891, #5745, #2645, #8326, #7783, #2559, #5120, #2598, #4523, #7103, #5922, #3479, #8038, #7873 ),
 .UNSPECIFIED., .F., .F.,
 ( 4, 2, 2, 2, 2, 2, 2, 2, 2, 2, 2, 2, 2, 2, 2, 4 ),
 ( 0.01224977136307512857, 0.01231928787409572804, 0.01238880438511632751, 0.01252783740715752644, 0.01280590345123992606, 0.01336203553940472182, 0.01447429971573431680, 0.01503043180389911429, 0.01558656389206391005, 0.01669882806839350503, 0.01725496015655830079, 0.01781109224472309654, 0.01836722433288789230, 0.01892335642105269153, 0.02003562059738228651, 0.02114788477371187803 ),
 .UNSPECIFIED. ) ;
#1271 = FACE_OUTER_BOUND ( 'NONE', #6683, .T. ) ;
#1272 = SURFACE_STYLE_FILL_AREA ( #3170 ) ;
#1273 = CARTESIAN_POINT ( 'NONE',  ( -2.493201789345250052, -91.05452850542926058, 1.934965279058294518 ) ) ;
#1274 = CARTESIAN_POINT ( 'NONE',  ( 7.360235569667875843, -61.24547149457073658, 0.09995255151716216091 ) ) ;
#1275 = DIRECTION ( 'NONE',  ( 0.000000000000000000, -1.000000000000000000, -1.734723475976807094E-16 ) ) ;
#1276 = CARTESIAN_POINT ( 'NONE',  ( 0.09506052544075337118, -61.99547149457074369, -4.999999999999997335 ) ) ;
#1277 = CARTESIAN_POINT ( 'NONE',  ( 5.895805022753498825, -96.94547149457073942, 4.407101234057782868 ) ) ;
#1278 = CARTESIAN_POINT ( 'NONE',  ( 55.00000000000000000, -25.00000000000002132, 20.00000000000000000 ) ) ;
#1279 = CARTESIAN_POINT ( 'NONE',  ( -80.00000000000000000, -19.99999999999999645, -12.50000000000000355 ) ) ;
#1280 = CARTESIAN_POINT ( 'NONE',  ( 0.09506052544085971667, -73.50452850542924921, 4.999999999999997335 ) ) ;
#1281 = CARTESIAN_POINT ( 'NONE',  ( 6.686770931921479644, -88.39547149457074227, -2.072711028461788896 ) ) ;
#1282 = EDGE_LOOP ( 'NONE', ( #2510, #7406, #1561, #794 ) ) ;
#1283 = DIRECTION ( 'NONE',  ( 0.000000000000000000, 0.000000000000000000, 1.000000000000000000 ) ) ;
#1284 = EDGE_CURVE ( 'NONE', #6465, #5374, #5993, .T. ) ;
#1285 = ORIENTED_EDGE ( 'NONE', *, *, #6456, .T. ) ;
#1286 = DIRECTION ( 'NONE',  ( 1.000000000000000000, 0.000000000000000000, -0.000000000000000000 ) ) ;
#1287 = CARTESIAN_POINT ( 'NONE',  ( -4.784657899331190123, -78.60452850542925773, -1.454677039711773867 ) ) ;
#1288 = CARTESIAN_POINT ( 'NONE',  ( -4.312004677470992142, -81.04547149457070532, 3.009306630940933758 ) ) ;
#1289 = EDGE_CURVE ( 'NONE', #5070, #3705, #5351, .T. ) ;
#1290 = DIRECTION ( 'NONE',  ( 0.000000000000000000, 0.000000000000000000, 1.000000000000000000 ) ) ;
#1291 = CARTESIAN_POINT ( 'NONE',  ( -0.09506052544075743738, -69.49547149457075079, 2.999999999999997780 ) ) ;
#1292 = CARTESIAN_POINT ( 'NONE',  ( 5.895805022753404678, -65.55452850542926058, -4.407101234057908989 ) ) ;
#1293 = CARTESIAN_POINT ( 'NONE',  ( 1.719659006605286367, -82.84547149457074511, -4.969112962950050338 ) ) ;
#1294 = CARTESIAN_POINT ( 'NONE',  ( 46.49999999999999289, -14.99999999999999467, 9.499999999999996447 ) ) ;
#1295 = CARTESIAN_POINT ( 'NONE',  ( 1.719659006605392504, -91.65452850542925489, 4.969112962950016588 ) ) ;
#1296 = CARTESIAN_POINT ( 'NONE',  ( 2.369498399071224615, -70.65452850542925489, 6.969112962950009482 ) ) ;
#1297 = CARTESIAN_POINT ( 'NONE',  ( 2.823794231030061663, -91.09547149457074511, 1.017458915287723809 ) ) ;
#1298 = ORIENTED_EDGE ( 'NONE', *, *, #7183, .T. ) ;
#1299 = CARTESIAN_POINT ( 'NONE',  ( 80.00000000000000000, 1.734723475976807094E-15, -12.50000000000000000 ) ) ;
#1300 = LINE ( 'NONE', #619, #716 ) ;
#1301 = CARTESIAN_POINT ( 'NONE',  ( 4.784657899331211439, -86.10452850542925773, 1.454677039711774533 ) ) ;
#1302 = ORIENTED_EDGE ( 'NONE', *, *, #3633, .T. ) ;
#1303 = CARTESIAN_POINT ( 'NONE',  ( 1.719659006605390950, -76.65452850542924068, 4.969112962950015699 ) ) ;
#1304 = CARTESIAN_POINT ( 'NONE',  ( -2.882544866740879286, -60.60452850542926484, -0.8366430509618996147 ) ) ;
#1305 = CARTESIAN_POINT ( 'NONE',  ( 1.719659006605391616, -82.65452850542925489, 4.969112962950016588 ) ) ;
#1306 = CARTESIAN_POINT ( 'NONE',  ( 0.09506052544073274879, -64.99547149457075079, -6.999999999999997335 ) ) ;
#1307 = CARTESIAN_POINT ( 'NONE',  ( -1.719659006605264606, -84.34547149457073090, 4.969112962950051227 ) ) ;
#1308 = CARTESIAN_POINT ( 'NONE',  ( 0.8796985632578985248, -71.85452850542924352, -3.030887037049972310 ) ) ;
#1309 = APPLICATION_CONTEXT ( 'automotive_design' ) ;
#1310 = PLANE ( 'NONE',  #6178 ) ;
#1311 = DIRECTION ( 'NONE',  ( 0.000000000000000000, -1.000000000000000000, 8.673617379884033007E-17 ) ) ;
#1312 = CARTESIAN_POINT ( 'NONE',  ( 1.069819614139558839, -91.65452850542924068, 2.969112962950023249 ) ) ;
#1313 = CARTESIAN_POINT ( 'NONE',  ( -2.179377348189613262, -59.14547149457074227, -7.030887037049939003 ) ) ;
#1314 = LINE ( 'NONE', #3886, #1466 ) ;
#1315 = CARTESIAN_POINT ( 'NONE',  ( -3.015831842038215527, -72.30452850542926058, -3.989209796945429432 ) ) ;
#1316 = CARTESIAN_POINT ( 'NONE',  ( 4.725907263620371168, -61.09547149457074511, 1.635492904037598283 ) ) ;
#1317 = DIRECTION ( 'NONE',  ( -0.000000000000000000, 0.7071067811865484609, -0.7071067811865465735 ) ) ;
#1318 = LINE ( 'NONE', #3891, #25 ) ;
#1319 = CARTESIAN_POINT ( 'NONE',  ( 4.312004677471073855, -58.95452850542925205, 3.009306630940844496 ) ) ;
#1320 = EDGE_CURVE ( 'NONE', #9, #5499, #4213, .T. ) ;
#1321 = CARTESIAN_POINT ( 'NONE',  ( 2.179377348189630581, -87.64547149457075648, 7.030887037049939003 ) ) ;
#1322 = ORIENTED_EDGE ( 'NONE', *, *, #7893, .T. ) ;
#1323 = CARTESIAN_POINT ( 'NONE',  ( 3.015831842038233734, -73.80452850542926058, 3.989209796945429432 ) ) ;
#1324 = CARTESIAN_POINT ( 'NONE',  ( 80.00000000000000000, -25.00000000000000000, -20.00000000000000000 ) ) ;
#1325 = CIRCLE ( 'NONE', #4616, 1.500000000000000666 ) ;
#1326 = DIRECTION ( 'NONE',  ( 1.000000000000000000, 0.000000000000000000, -0.000000000000000000 ) ) ;
#1327 = CARTESIAN_POINT ( 'NONE',  ( 4.725907263620373833, -82.09547149457074511, 1.635492904037598283 ) ) ;
#1328 = VECTOR ( 'NONE', #5772, 1000.000000000000000 ) ;
#1329 = DIRECTION ( 'NONE',  ( 0.000000000000000000, -0.000000000000000000, -1.000000000000000000 ) ) ;
#1330 = CARTESIAN_POINT ( 'NONE',  ( 1.840261337453219959, -73.69547149457073942, -2.371175808195584267 ) ) ;
#1331 = VECTOR ( 'NONE', #6015, 1000.000000000000114 ) ;
#1332 = CARTESIAN_POINT ( 'NONE',  ( 7.360235569667877620, -68.25452850542924921, -0.09995255151731691212 ) ) ;
#1333 = LINE ( 'NONE', #4608, #1729 ) ;
#1334 = CARTESIAN_POINT ( 'NONE',  ( 3.015831842038149802, -82.69547149457073942, -3.989209796945492048 ) ) ;
#1335 = CARTESIAN_POINT ( 'NONE',  ( 4.784657899331207886, -59.10452850542925773, 1.454677039711774533 ) ) ;
#1336 = LINE ( 'NONE', #1935, #7777 ) ;
#1337 = CARTESIAN_POINT ( 'NONE',  ( 7.360235569667877620, -68.25452850542924921, -0.09995255151731691212 ) ) ;
#1338 = VECTOR ( 'NONE', #7478, 1000.000000000000000 ) ;
#1339 = PRESENTATION_LAYER_ASSIGNMENT (  '', '', ( #7399 ) ) ;
#1340 = CARTESIAN_POINT ( 'NONE',  ( -1.840261337453199975, -81.19547149457073942, 2.371175808195584267 ) ) ;
#1341 = VERTEX_POINT ( 'NONE', #6664 ) ;
#1342 = LINE ( 'NONE', #702, #2282 ) ;
#1343 = CARTESIAN_POINT ( 'NONE',  ( 1.719659006605392504, -94.65452850542921226, 4.969112962950016588 ) ) ;
#1344 = CARTESIAN_POINT ( 'NONE',  ( 4.194503406049338246, -83.55452850542921794, -3.171033256558100089 ) ) ;
#1345 = ORIENTED_EDGE ( 'NONE', *, *, #2125, .T. ) ;
#1346 = CARTESIAN_POINT ( 'NONE',  ( 4.312004677471078296, -82.95452850542925205, 3.009306630940844052 ) ) ;
#1347 = CARTESIAN_POINT ( 'NONE',  ( 2.882544866740894385, -59.10452850542926484, 0.8366430509618999478 ) ) ;
#1348 = AXIS2_PLACEMENT_3D ( 'NONE', #6049, #867, #2180 ) ;
#1349 = CARTESIAN_POINT ( 'NONE',  ( -4.725907263620320542, -84.90452850542925489, 1.635492904037698647 ) ) ;
#1350 = CARTESIAN_POINT ( 'NONE',  ( 4.037591185471560706, -63.79547149457074084, 5.718994135553860936 ) ) ;
#1351 = CARTESIAN_POINT ( 'NONE',  ( -4.194503406049383543, -80.44547149457073942, -3.171033256558012159 ) ) ;
#1352 = CARTESIAN_POINT ( 'NONE',  ( 2.823794231030039015, -65.40452850542925489, -1.017458915287783316 ) ) ;
#1353 = MECHANICAL_DESIGN_GEOMETRIC_PRESENTATION_REPRESENTATION (  '', ( #7140 ), #3380 ) ;
#1354 = CARTESIAN_POINT ( 'NONE',  ( 6.123233995736760366E-16, -26.99999999999998934, 0.000000000000000000 ) ) ;
#1355 = LINE ( 'NONE', #5898, #2705 ) ;
#1356 = CARTESIAN_POINT ( 'NONE',  ( 2.823794231030042567, -92.40452850542925489, -1.017458915287783316 ) ) ;
#1357 = CARTESIAN_POINT ( 'NONE',  ( 2.179377348189627472, -60.64547149457074227, 7.030887037049939003 ) ) ;
#1358 = EDGE_CURVE ( 'NONE', #8122, #577, #2207, .T. ) ;
#1359 = CARTESIAN_POINT ( 'NONE',  ( 47.50000000000002132, -54.00000000000000711, 12.50000000000001954 ) ) ;
#1360 = CARTESIAN_POINT ( 'NONE',  ( -5.257311121191323267, -81.75452850542926342, 0.09995255151729526277 ) ) ;
#1361 = CARTESIAN_POINT ( 'NONE',  ( 4.191402346623079644, -85.69547149457073942, -5.607243785695398941 ) ) ;
#1362 = FACE_OUTER_BOUND ( 'NONE', #455, .T. ) ;
#1363 = PLANE ( 'NONE',  #7305 ) ;
#1364 = CARTESIAN_POINT ( 'NONE',  ( 4.194503406049334693, -59.55452850542926058, -3.171033256558100089 ) ) ;
#1365 = CARTESIAN_POINT ( 'NONE',  ( -7.360235569667858080, -86.74547149457075079, -0.09995255151716124498 ) ) ;
#1366 =( LENGTH_UNIT ( ) NAMED_UNIT ( * ) SI_UNIT ( .MILLI., .METRE. ) );
#1367 = EDGE_LOOP ( 'NONE', ( #750, #4824, #5261, #5007 ) ) ;
#1368 = CARTESIAN_POINT ( 'NONE',  ( 4.194503406049337357, -74.55452850542923215, -3.171033256558100089 ) ) ;
#1369 = DIRECTION ( 'NONE',  ( 1.000000000000000000, -0.000000000000000000, -0.000000000000000000 ) ) ;
#1370 = CARTESIAN_POINT ( 'NONE',  ( -80.00000000000000000, 0.000000000000000000, 20.00000000000000000 ) ) ;
#1371 = CARTESIAN_POINT ( 'NONE',  ( 1.719659006605286145, -79.84547149457071669, -4.969112962950050338 ) ) ;
#1372 = DIRECTION ( 'NONE',  ( -0.000000000000000000, -0.000000000000000000, 1.000000000000000000 ) ) ;
#1373 = CARTESIAN_POINT ( 'NONE',  ( 0.09506052544075790922, -97.99547149457075079, -4.999999999999997335 ) ) ;
#1374 = CARTESIAN_POINT ( 'NONE',  ( -0.09506052544086177059, -72.00452850542926342, -6.999999999999997335 ) ) ;
#1375 = DIRECTION ( 'NONE',  ( -1.000000000000000000, -0.000000000000000000, -0.000000000000000000 ) ) ;
#1376 = CARTESIAN_POINT ( 'NONE',  ( 3.015831842038148913, -76.69547149457075363, -3.989209796945492048 ) ) ;
#1377 = CARTESIAN_POINT ( 'NONE',  ( 4.302742873392585210, -96.99999999999947420, 2.548615363087012753 ) ) ;
#1378 = CARTESIAN_POINT ( 'NONE',  ( -3.015831842038213750, -87.30452850542926058, -3.989209796945429432 ) ) ;
#1379 = CARTESIAN_POINT ( 'NONE',  ( -4.191402346623180009, -66.30452850542926058, -5.607243785695311900 ) ) ;
#1380 = CARTESIAN_POINT ( 'NONE',  ( -1.069819614139474462, -78.34547149457074511, 2.969112962950044121 ) ) ;
#1381 = VERTEX_POINT ( 'NONE', #5356 ) ;
#1382 = FACE_OUTER_BOUND ( 'NONE', #7336, .T. ) ;
#1383 = DIRECTION ( 'NONE',  ( -0.000000000000000000, 2.775557561562891351E-16, -1.000000000000000000 ) ) ;
#1384 = CARTESIAN_POINT ( 'NONE',  ( 3.015831842038235067, -85.80452850542926058, 3.989209796945429432 ) ) ;
#1385 = ORIENTED_EDGE ( 'NONE', *, *, #8097, .T. ) ;
#1386 = CARTESIAN_POINT ( 'NONE',  ( 4.784657899331210551, -83.10452850542927195, 1.454677039711774533 ) ) ;
#1387 = CARTESIAN_POINT ( 'NONE',  ( 1.840261337453221957, -91.69547149457075363, -2.371175808195584267 ) ) ;
#1388 = CARTESIAN_POINT ( 'NONE',  ( -31.55601659751036792, 8.414937759336103440, -2.499999999999998668 ) ) ;
#1389 = CARTESIAN_POINT ( 'NONE',  ( 4.312004677471076519, -82.95452850542925205, 3.009306630940844496 ) ) ;
#1390 = CARTESIAN_POINT ( 'NONE',  ( 7.360235569667875843, -61.24547149457073658, 0.09995255151716216091 ) ) ;
#1391 = CARTESIAN_POINT ( 'NONE',  ( 0.09506052544083769262, -67.50452850542926342, 2.999999999999997780 ) ) ;
#1392 = PRODUCT_DEFINITION ( 'UNKNOWN', '', #2424, #5360 ) ;
#1393 = LINE ( 'NONE', #3386, #802 ) ;
#1394 = PLANE ( 'NONE',  #6055 ) ;
#1395 = CARTESIAN_POINT ( 'NONE',  ( -0.09506052544081818045, -84.00452850542926342, -2.999999999999997780 ) ) ;
#1396 = AXIS2_PLACEMENT_3D ( 'NONE', #877, #2027, #3452 ) ;
#1397 = CARTESIAN_POINT ( 'NONE',  ( -4.037591185471420374, -94.20452850542928047, 5.718994135553947977 ) ) ;
#1398 = AXIS2_PLACEMENT_3D ( 'NONE', #5158, #2596, #5786 ) ;
#1399 = DIRECTION ( 'NONE',  ( -0.000000000000000000, -0.000000000000000000, -1.000000000000000000 ) ) ;
#1400 = CARTESIAN_POINT ( 'NONE',  ( 4.194503406049337357, -77.55452850542926058, -3.171033256558100089 ) ) ;
#1401 = CARTESIAN_POINT ( 'NONE',  ( -5.895805022753476621, -86.44547149457073942, -4.407101234057782868 ) ) ;
#1402 = DIRECTION ( 'NONE',  ( -1.000000000000000000, 0.000000000000000000, 0.000000000000000000 ) ) ;
#1403 = DIRECTION ( 'NONE',  ( -1.000000000000000000, 0.000000000000000000, -0.000000000000000000 ) ) ;
#1404 = CARTESIAN_POINT ( 'NONE',  ( 0.8796985632579609193, -69.64547149457072805, 3.030887037049952326 ) ) ;
#1405 = EDGE_CURVE ( 'NONE', #4928, #2966, #379, .T. ) ;
#1406 = CARTESIAN_POINT ( 'NONE',  ( 1.719659006605388507, -61.65452850542923358, 4.969112962950016588 ) ) ;
#1407 = CARTESIAN_POINT ( 'NONE',  ( 7.360235569667880284, -94.24547149457075079, 0.09995255151716216091 ) ) ;
#1408 = COLOUR_RGB ( '', 0.66274510, 0.83137255, 0.94901961) ;
#1409 =( LENGTH_UNIT ( ) NAMED_UNIT ( * ) SI_UNIT ( .MILLI., .METRE. ) );
#1410 = ORIENTED_EDGE ( 'NONE', *, *, #4273, .F. ) ;
#1411 = CARTESIAN_POINT ( 'NONE',  ( 3.015831842038233290, -70.80452850542926058, 3.989209796945429432 ) ) ;
#1412 = DIRECTION ( 'NONE',  ( 1.000000000000000000, 9.251858538542971581E-17, 1.604941620322696727E-32 ) ) ;
#1413 = VECTOR ( 'NONE', #2847, 1000.000000000000000 ) ;
#1414 = DIRECTION ( 'NONE',  ( -0.000000000000000000, -3.469446951953614682E-16, -1.000000000000000000 ) ) ;
#1415 = CARTESIAN_POINT ( 'NONE',  ( -4.194503406049384431, -77.44547149457075363, -3.171033256558012159 ) ) ;
#1416 = CARTESIAN_POINT ( 'NONE',  ( 4.302742873392585210, -96.99999999999947420, 2.548615363087012753 ) ) ;
#1417 = CARTESIAN_POINT ( 'NONE',  ( 3.015831842038151578, -97.69547149457075363, -3.989209796945492048 ) ) ;
#1418 = CARTESIAN_POINT ( 'NONE',  ( 2.369498399071224615, -70.65452850542925489, 6.969112962950009482 ) ) ;
#1419 = DIRECTION ( 'NONE',  ( -1.000000000000000000, -0.000000000000000000, -0.000000000000000000 ) ) ;
#1420 = CARTESIAN_POINT ( 'NONE',  ( 4.725907263620372945, -79.09547149457074511, 1.635492904037598283 ) ) ;
#1421 = APPLICATION_CONTEXT ( 'automotive_design' ) ;
#1422 = CARTESIAN_POINT ( 'NONE',  ( -65.00000000000000000, -7.999999999999996447, 12.49999999999999822 ) ) ;
#1423 = CARTESIAN_POINT ( 'NONE',  ( -3.015831842038213750, -84.30452850542926058, -3.989209796945429432 ) ) ;
#1424 = CARTESIAN_POINT ( 'NONE',  ( -5.895805022753386915, -67.05452850542926058, 4.407101234057909878 ) ) ;
#1425 = CARTESIAN_POINT ( 'NONE',  ( 0.8796985632579621406, -78.64547149457074227, 3.030887037049952326 ) ) ;
#1426 = EDGE_CURVE ( 'NONE', #4198, #4887, #2956, .T. ) ;
#1427 = ORIENTED_EDGE ( 'NONE', *, *, #3922, .F. ) ;
#1428 = CARTESIAN_POINT ( 'NONE',  ( 45.00000000000000000, -14.99999999999999467, 2.500000000000000888 ) ) ;
#1429 = DIRECTION ( 'NONE',  ( 0.000000000000000000, 0.000000000000000000, 1.000000000000000000 ) ) ;
#1430 = CARTESIAN_POINT ( 'NONE',  ( -4.194503406049315153, -91.05452850542923215, 3.171033256558100533 ) ) ;
#1431 = ORIENTED_EDGE ( 'NONE', *, *, #1570, .T. ) ;
#1432 = CARTESIAN_POINT ( 'NONE',  ( -4.194503406049316929, -82.05452850542926058, 3.171033256558101865 ) ) ;
#1433 = CARTESIAN_POINT ( 'NONE',  ( 0.09506052544077819855, -91.99547149457075079, -2.999999999999997780 ) ) ;
#1434 = DIRECTION ( 'NONE',  ( -0.000000000000000000, -0.000000000000000000, -1.000000000000000000 ) ) ;
#1435 = CARTESIAN_POINT ( 'NONE',  ( -4.725907263620320542, -81.90452850542925489, 1.635492904037698647 ) ) ;
#1436 = CARTESIAN_POINT ( 'NONE',  ( -6.686770931921503625, -93.60452850542925773, -2.072711028461647675 ) ) ;
#1437 = CARTESIAN_POINT ( 'NONE',  ( 2.610703060766982553, -67.95452850542925205, 1.773238653441072232 ) ) ;
#1438 = CARTESIAN_POINT ( 'NONE',  ( -80.00000000000000000, 2.168404344971008868E-15, -12.50000000000000000 ) ) ;
#1439 = DIRECTION ( 'NONE',  ( 0.000000000000000000, 0.000000000000000000, -1.000000000000000000 ) ) ;
#1440 = CARTESIAN_POINT ( 'NONE',  ( -2.610703060766964345, -78.45452850542925205, -1.773238653441072232 ) ) ;
#1441 = CARTESIAN_POINT ( 'NONE',  ( 7.360235569667880284, -89.25452850542926342, -0.09995255151731691212 ) ) ;
#1442 = DIRECTION ( 'NONE',  ( -0.000000000000000000, -0.000000000000000000, 1.000000000000000000 ) ) ;
#1443 = CARTESIAN_POINT ( 'NONE',  ( 5.895805022753496161, -87.94547149457073942, 4.407101234057782868 ) ) ;
#1444 = DIRECTION ( 'NONE',  ( 1.000000000000000000, 0.000000000000000000, 0.000000000000000000 ) ) ;
#1445 = LINE ( 'NONE', #2167, #3270 ) ;
#1446 = CARTESIAN_POINT ( 'NONE',  ( 2.610703060766944361, -70.54547149457074795, -1.773238653441125523 ) ) ;
#1447 = ORIENTED_EDGE ( 'NONE', *, *, #5442, .T. ) ;
#1448 = CARTESIAN_POINT ( 'NONE',  ( -4.725907263620322318, -66.90452850542925489, 1.635492904037698647 ) ) ;
#1449 = CARTESIAN_POINT ( 'NONE',  ( -0.09506052544071380561, -78.49547149457075079, 6.999999999999997335 ) ) ;
#1450 = VERTEX_POINT ( 'NONE', #893 ) ;
#1451 = VECTOR ( 'NONE', #6786, 1000.000000000000000 ) ;
#1452 = CARTESIAN_POINT ( 'NONE',  ( 2.862020680886514512, -77.70452850542926626, -4.100960146804039752 ) ) ;
#1453 = LINE ( 'NONE', #6594, #5169 ) ;
#1454 = CONTEXT_DEPENDENT_SHAPE_REPRESENTATION ( #4869, #1107 ) ;
#1455 = CARTESIAN_POINT ( 'NONE',  ( 2.862020680886599777, -81.79547149457073374, 4.100960146803977580 ) ) ;
#1456 = LINE ( 'NONE', #4028, #3228 ) ;
#1457 = CARTESIAN_POINT ( 'NONE',  ( 0.8796985632579601422, -63.64547149457072805, 3.030887037049952326 ) ) ;
#1458 = CARTESIAN_POINT ( 'NONE',  ( 2.369498399071224615, -73.65452850542925489, 6.969112962950009482 ) ) ;
#1459 = DIRECTION ( 'NONE',  ( 0.000000000000000000, 1.000000000000000000, 0.000000000000000000 ) ) ;
#1460 = ADVANCED_FACE ( 'NONE', ( #934 ), #3467, .F. ) ;
#1461 = DIRECTION ( 'NONE',  ( 0.000000000000000000, -0.000000000000000000, 1.000000000000000000 ) ) ;
#1462 = CARTESIAN_POINT ( 'NONE',  ( -2.862020680886493640, -82.20452850542925205, 4.100960146804039752 ) ) ;
#1463 = CARTESIAN_POINT ( 'NONE',  ( -6.013306294175152722, -69.45452850542925205, -4.245374608440613429 ) ) ;
#1464 = ADVANCED_FACE ( 'NONE', ( #7342 ), #4174, .T. ) ;
#1465 = CARTESIAN_POINT ( 'NONE',  ( 2.882544866740877954, -82.39547149457074227, -0.8366430509619593447 ) ) ;
#1466 = VECTOR ( 'NONE', #1275, 1000.000000000000000 ) ;
#1467 = ORIENTED_EDGE ( 'NONE', *, *, #3107, .T. ) ;
#1468 = AXIS2_PLACEMENT_3D ( 'NONE', #3072, #1220, #4965 ) ;
#1469 = CARTESIAN_POINT ( 'NONE',  ( -6.000000000000007105, -51.00000000000000711, 2.500000000000000888 ) ) ;
#1470 = DIRECTION ( 'NONE',  ( -0.000000000000000000, -0.000000000000000000, -1.000000000000000000 ) ) ;
#1471 = CARTESIAN_POINT ( 'NONE',  ( -4.725907263620319654, -90.90452850542926910, 1.635492904037698647 ) ) ;
#1472 = ORIENTED_EDGE ( 'NONE', *, *, #5256, .T. ) ;
#1473 = CARTESIAN_POINT ( 'NONE',  ( -4.194503406049317817, -73.05452850542926058, 3.171033256558101865 ) ) ;
#1474 = CARTESIAN_POINT ( 'NONE',  ( -0.09506052544075518917, -87.49547149457075079, 2.999999999999997780 ) ) ;
#1475 = CARTESIAN_POINT ( 'NONE',  ( 4.725907263620341858, -86.40452850542926910, -1.635492904037697981 ) ) ;
#1476 = MECHANICAL_DESIGN_GEOMETRIC_PRESENTATION_REPRESENTATION (  '', ( #7399 ), #3358 ) ;
#1477 = CARTESIAN_POINT ( 'NONE',  ( 7.360235569667875843, -64.24547149457075079, 0.09995255151716216091 ) ) ;
#1478 = AXIS2_PLACEMENT_3D ( 'NONE', #7633, #1869, #590 ) ;
#1479 = CARTESIAN_POINT ( 'NONE',  ( 3.154386672714807549, -68.25452850542924921, -0.09995255151727241993 ) ) ;
#1480 = CARTESIAN_POINT ( 'NONE',  ( 0.000000000000000000, -9.999999999999994671, 0.000000000000000000 ) ) ;
#1481 = AXIS2_PLACEMENT_3D ( 'NONE', #6071, #6783, #2872 ) ;
#1482 = LINE ( 'NONE', #628, #7816 ) ;
#1483 = CARTESIAN_POINT ( 'NONE',  ( -2.610703060766965233, -75.45452850542925205, -1.773238653441072232 ) ) ;
#1484 = CARTESIAN_POINT ( 'NONE',  ( -6.013306294175149169, -93.45452850542926626, -4.245374608440613429 ) ) ;
#1485 = CARTESIAN_POINT ( 'NONE',  ( -2.179377348189609265, -89.14547149457072805, -7.030887037049939003 ) ) ;
#1486 = FACE_OUTER_BOUND ( 'NONE', #1815, .T. ) ;
#1487 = CARTESIAN_POINT ( 'NONE',  ( 80.00000000000000000, -1.734723475976807094E-15, 12.50000000000000000 ) ) ;
#1488 = CARTESIAN_POINT ( 'NONE',  ( 1.686450176301634851, -66.79547149457073374, 2.482926158054096000 ) ) ;
#1489 = EDGE_CURVE ( 'NONE', #140, #2962, #8023, .T. ) ;
#1490 = VERTEX_POINT ( 'NONE', #5600 ) ;
#1491 = CARTESIAN_POINT ( 'NONE',  ( 4.312004677471074743, -70.95452850542925205, 3.009306630940844496 ) ) ;
#1492 = CARTESIAN_POINT ( 'NONE',  ( -6.013306294175058575, -81.04547149457074795, 4.245374608440741326 ) ) ;
#1493 =( NAMED_UNIT ( * ) PLANE_ANGLE_UNIT ( ) SI_UNIT ( $, .RADIAN. ) );
#1494 = ORIENTED_EDGE ( 'NONE', *, *, #7223, .T. ) ;
#1495 = CARTESIAN_POINT ( 'NONE',  ( -4.312004677471057867, -75.45452850542925205, -3.009306630940844052 ) ) ;
#1496 = CARTESIAN_POINT ( 'NONE',  ( -4.481820730511953954E-14, -57.99999999999999289, -4.999999999999997335 ) ) ;
#1497 = PRODUCT_DEFINITION ( 'UNKNOWN', '', #7527, #7983 ) ;
#1498 = CARTESIAN_POINT ( 'NONE',  ( -5.257311121191324155, -68.74547149457072237, -0.09995255151718371311 ) ) ;
#1499 = LINE ( 'NONE', #1630, #2833 ) ;
#1500 = CARTESIAN_POINT ( 'NONE',  ( -1.719659006605263496, -96.34547149457074511, 4.969112962950051227 ) ) ;
#1501 = CARTESIAN_POINT ( 'NONE',  ( 5.895805022753402902, -62.55452850542925347, -4.407101234057908989 ) ) ;
#1502 = FACE_OUTER_BOUND ( 'NONE', #6943, .T. ) ;
#1503 = SURFACE_STYLE_FILL_AREA ( #278 ) ;
#1504 = CARTESIAN_POINT ( 'NONE',  ( 4.725907263620341858, -86.40452850542926910, -1.635492904037697981 ) ) ;
#1505 = CARTESIAN_POINT ( 'NONE',  ( 5.895805022753402902, -62.55452850542925347, -4.407101234057908989 ) ) ;
#1506 = CARTESIAN_POINT ( 'NONE',  ( -3.154386672714789785, -77.74547149457073658, -0.09995255151720625064 ) ) ;
#1507 = ORIENTED_EDGE ( 'NONE', *, *, #1229, .T. ) ;
#1508 = CARTESIAN_POINT ( 'NONE',  ( 80.00000000000000000, -12.00000000000000355, -12.50000000000000178 ) ) ;
#1509 = CARTESIAN_POINT ( 'NONE',  ( 5.257311121191342806, -92.25452850542922079, -0.09995255151729465215 ) ) ;
#1510 = CARTESIAN_POINT ( 'NONE',  ( 4.312004677471076519, -79.95452850542922363, 3.009306630940844496 ) ) ;
#1511 = ORIENTED_EDGE ( 'NONE', *, *, #6199, .T. ) ;
#1512 = CARTESIAN_POINT ( 'NONE',  ( 5.257311121191341030, -68.25452850542926342, -0.09995255151729466603 ) ) ;
#1513 = CARTESIAN_POINT ( 'NONE',  ( -3.154386672714788453, -86.74547149457075079, -0.09995255151720625064 ) ) ;
#1514 = ADVANCED_FACE ( 'NONE', ( #4972 ), #1737, .F. ) ;
#1515 = CARTESIAN_POINT ( 'NONE',  ( -3.154386672714792006, -62.74547149457073658, -0.09995255151720625064 ) ) ;
#1516 = CARTESIAN_POINT ( 'NONE',  ( -6.013306294175061240, -63.04547149457074084, 4.245374608440741326 ) ) ;
#1517 = CARTESIAN_POINT ( 'NONE',  ( 1.840261337453268808, -61.80452850542926058, 2.371175808195547852 ) ) ;
#1518 = AXIS2_PLACEMENT_3D ( 'NONE', #682, #3093, #6 ) ;
#1520 = EDGE_CURVE ( 'NONE', #5848, #6118, #2330, .T. ) ;
#1519 = ORIENTED_EDGE ( 'NONE', *, *, #4696, .F. ) ;
#1521 = DIRECTION ( 'NONE',  ( -1.000000000000000000, 0.000000000000000000, 0.000000000000000000 ) ) ;
#1522 = FACE_OUTER_BOUND ( 'NONE', #685, .T. ) ;
#1523 = CARTESIAN_POINT ( 'NONE',  ( 0.09506052544083919142, -79.50452850542926342, 2.999999999999997780 ) ) ;
#1524 = CARTESIAN_POINT ( 'NONE',  ( 6.686770931921525829, -86.10452850542924352, 2.072711028461649008 ) ) ;
#1525 = CARTESIAN_POINT ( 'NONE',  ( -2.369498399071056305, -84.34547149457075932, 6.969112962950058332 ) ) ;
#1526 = DIRECTION ( 'NONE',  ( -0.000000000000000000, -8.673617379884033007E-17, -1.000000000000000000 ) ) ;
#1527 = DIRECTION ( 'NONE',  ( 1.000000000000000000, -0.000000000000000000, -0.000000000000000000 ) ) ;
#1528 = CARTESIAN_POINT ( 'NONE',  ( -2.823794231030041235, -65.59547149457073090, -1.017458915287723364 ) ) ;
#1529 = AXIS2_PLACEMENT_3D ( 'NONE', #201, #8044, #239 ) ;
#1530 = VERTEX_POINT ( 'NONE', #3713 ) ;
#1531 = CARTESIAN_POINT ( 'NONE',  ( -1.719659006605373630, -66.15452850542926910, -4.969112962950016588 ) ) ;
#1532 = CARTESIAN_POINT ( 'NONE',  ( -6.686770931921458327, -83.89547149457074227, 2.072711028461789784 ) ) ;
#1533 = ORIENTED_EDGE ( 'NONE', *, *, #7718, .F. ) ;
#1534 = CIRCLE ( 'NONE', #5828, 4.000000000000000000 ) ;
#1535 = CARTESIAN_POINT ( 'NONE',  ( 1.719659006605389617, -67.65452850542925489, 4.969112962950016588 ) ) ;
#1536 = VECTOR ( 'NONE', #1470, 1000.000000000000000 ) ;
#1537 = FACE_OUTER_BOUND ( 'NONE', #1693, .T. ) ;
#1538 = AXIS2_PLACEMENT_3D ( 'NONE', #2727, #3719, #7552 ) ;
#1539 = AXIS2_PLACEMENT_3D ( 'NONE', #6210, #4308, #8076 ) ;
#1540 = CARTESIAN_POINT ( 'NONE',  ( -4.312004677470993919, -69.04547149457071953, 3.009306630940933758 ) ) ;
#1541 = CARTESIAN_POINT ( 'NONE',  ( 45.00000000000000000, -14.99999999999999467, 4.500000000000000888 ) ) ;
#1542 = CARTESIAN_POINT ( 'NONE',  ( 0.09506052544077440991, -61.99547149457073658, -2.999999999999997780 ) ) ;
#1543 = CARTESIAN_POINT ( 'NONE',  ( -0.09506052544086329714, -60.00452850542925631, -6.999999999999997335 ) ) ;
#1544 = EDGE_LOOP ( 'NONE', ( #2817, #1646, #7710, #7360 ) ) ;
#1545 = EDGE_CURVE ( 'NONE', #2326, #3416, #2265, .T. ) ;
#1546 =( NAMED_UNIT ( * ) PLANE_ANGLE_UNIT ( ) SI_UNIT ( $, .RADIAN. ) );
#1547 = CARTESIAN_POINT ( 'NONE',  ( -3.015831842038213750, -90.30452850542926058, -3.989209796945429432 ) ) ;
#1548 = EDGE_CURVE ( 'NONE', #5519, #1381, #5167, .T. ) ;
#1549 = CLOSED_SHELL ( 'NONE', ( #879, #7015, #477, #7270, #2468, #1870, #1464, #4583, #5249, #6031, #2053, #5963, #7130, #6092, #5785, #960, #4435, #7621, #3038, #8204, #1159, #291, #8313, #7524, #5577, #7294, #6000 ) ) ;
#1550 = ORIENTED_EDGE ( 'NONE', *, *, #4901, .F. ) ;
#1551 = FACE_OUTER_BOUND ( 'NONE', #8281, .T. ) ;
#1552 = CARTESIAN_POINT ( 'NONE',  ( 1.719659006605392504, -91.65452850542925489, 4.969112962950016588 ) ) ;
#1553 = CARTESIAN_POINT ( 'NONE',  ( 3.015831842038234623, -82.80452850542926058, 3.989209796945429432 ) ) ;
#1554 = VERTEX_POINT ( 'NONE', #6477 ) ;
#1555 = CARTESIAN_POINT ( 'NONE',  ( -0.09506052544084034328, -75.00452850542924921, -4.999999999999997335 ) ) ;
#1556 = CARTESIAN_POINT ( 'NONE',  ( 2.882544866740878842, -88.39547149457074227, -0.8366430509619593447 ) ) ;
#1557 = CARTESIAN_POINT ( 'NONE',  ( 1.719659006605287477, -94.84547149457074511, -4.969112962950050338 ) ) ;
#1558 = CARTESIAN_POINT ( 'NONE',  ( -3.015831842038214194, -81.30452850542926058, -3.989209796945429432 ) ) ;
#1559 = CARTESIAN_POINT ( 'NONE',  ( 4.191402346623198660, -88.80452850542926058, 5.607243785695311900 ) ) ;
#1560 = CARTESIAN_POINT ( 'NONE',  ( -0.09506052544082159439, -57.00452850542925631, -2.999999999999997780 ) ) ;
#1561 = ORIENTED_EDGE ( 'NONE', *, *, #167, .F. ) ;
#1562 = DIRECTION ( 'NONE',  ( 0.000000000000000000, 0.000000000000000000, 1.000000000000000000 ) ) ;
#1563 = DIRECTION ( 'NONE',  ( 0.000000000000000000, -1.734723475976807094E-16, 1.000000000000000000 ) ) ;
#1564 = CARTESIAN_POINT ( 'NONE',  ( -1.686450176301565351, -79.20452850542925205, 2.482926158054133303 ) ) ;
#1565 = CARTESIAN_POINT ( 'NONE',  ( -0.09506052544085952238, -90.00452850542926342, -6.999999999999997335 ) ) ;
#1566 = CARTESIAN_POINT ( 'NONE',  ( -4.037591185471543831, -83.29547149457074795, -5.718994135553860936 ) ) ;
#1567 = DIRECTION ( 'NONE',  ( 0.000000000000000000, 1.000000000000000000, 1.734723475976807094E-16 ) ) ;
#1568 = CARTESIAN_POINT ( 'NONE',  ( -0.09506052544073276267, -96.49547149457075079, 4.999999999999997335 ) ) ;
#1569 = CARTESIAN_POINT ( 'NONE',  ( -1.840261337453200863, -72.19547149457073942, 2.371175808195584267 ) ) ;
#1570 = EDGE_CURVE ( 'NONE', #1136, #981, #7746, .T. ) ;
#1571 = UNCERTAINTY_MEASURE_WITH_UNIT (LENGTH_MEASURE( 1.000000000000000082E-05 ), #2347, 'distance_accuracy_value', 'NONE');
#1572 = LINE ( 'NONE', #6791, #7584 ) ;
#1573 = VERTEX_POINT ( 'NONE', #6434 ) ;
#1574 = CARTESIAN_POINT ( 'NONE',  ( 43.50000000000000711, -14.99999999999999467, 4.499999999999999112 ) ) ;
#1575 = CARTESIAN_POINT ( 'NONE',  ( -4.194503406049319594, -70.05452850542923215, 3.171033256558100533 ) ) ;
#1576 = CARTESIAN_POINT ( 'NONE',  ( -6.628020296210667794, -77.59547149457073090, -2.253526892787471869 ) ) ;
#1577 = DIRECTION ( 'NONE',  ( -9.251858538542971581E-17, 1.000000000000000000, -0.000000000000000000 ) ) ;
#1578 = CARTESIAN_POINT ( 'NONE',  ( 5.257311121191341030, -79.24547149457073658, 0.09995255151718437925 ) ) ;
#1579 = CARTESIAN_POINT ( 'NONE',  ( -2.862020680886580681, -74.29547149457074795, -4.100960146803977580 ) ) ;
#1580 = CARTESIAN_POINT ( 'NONE',  ( 1.719659006605389173, -64.65452850542925489, 4.969112962950016588 ) ) ;
#1581 = DIRECTION ( 'NONE',  ( 1.000000000000000000, 0.000000000000000000, 0.000000000000000000 ) ) ;
#1582 = EDGE_CURVE ( 'NONE', #7184, #3118, #1336, .T. ) ;
#1583 = CARTESIAN_POINT ( 'NONE',  ( -4.725907263620353405, -74.59547149457074511, -1.635492904037597617 ) ) ;
#1584 = AXIS2_PLACEMENT_3D ( 'NONE', #3847, #5275, #1444 ) ;
#1585 = DIRECTION ( 'NONE',  ( 0.000000000000000000, 0.000000000000000000, 1.000000000000000000 ) ) ;
#1586 = CARTESIAN_POINT ( 'NONE',  ( -5.895805022753386915, -58.05452850542925347, 4.407101234057909878 ) ) ;
#1587 = VERTEX_POINT ( 'NONE', #5125 ) ;
#1588 =( NAMED_UNIT ( * ) SI_UNIT ( $, .STERADIAN. ) SOLID_ANGLE_UNIT ( ) );
#1589 = ADVANCED_FACE ( 'NONE', ( #1057 ), #4779, .T. ) ;
#1590 = VERTEX_POINT ( 'NONE', #1377 ) ;
#1591 = DIRECTION ( 'NONE',  ( -0.6099942813304201072, -0.7924058156930603447, 0.000000000000000000 ) ) ;
#1592 = CARTESIAN_POINT ( 'NONE',  ( 5.257311121191342806, -89.25452850542924921, -0.09995255151729465215 ) ) ;
#1593 = CARTESIAN_POINT ( 'NONE',  ( -4.725907263620320542, -81.90452850542925489, 1.635492904037698647 ) ) ;
#1594 = VERTEX_POINT ( 'NONE', #6433 ) ;
#1595 = CARTESIAN_POINT ( 'NONE',  ( -4.725907263620322318, -69.90452850542925489, 1.635492904037698647 ) ) ;
#1596 = CARTESIAN_POINT ( 'NONE',  ( -0.8796985632579421566, -83.14547149457072805, -3.030887037049952326 ) ) ;
#1597 = CARTESIAN_POINT ( 'NONE',  ( -3.015831842038126709, -93.19547149457075363, 3.989209796945492048 ) ) ;
#1598 = CARTESIAN_POINT ( 'NONE',  ( 5.257311121191341918, -77.25452850542926342, -0.09995255151729465215 ) ) ;
#1599 = CARTESIAN_POINT ( 'NONE',  ( 5.895805022753407343, -89.55452850542926058, -4.407101234057908989 ) ) ;
#1600 = CARTESIAN_POINT ( 'NONE',  ( -3.154386672714792006, -57.75452850542924921, 0.09995255151727280851 ) ) ;
#1601 = VECTOR ( 'NONE', #2366, 1000.000000000000000 ) ;
#1602 = EDGE_LOOP ( 'NONE', ( #1188, #56, #2548, #7393 ) ) ;
#1603 = FACE_OUTER_BOUND ( 'NONE', #4496, .T. ) ;
#1604 = VECTOR ( 'NONE', #3130, 1000.000000000000000 ) ;
#1605 = CARTESIAN_POINT ( 'NONE',  ( 45.96623493960122886, -14.74233734943963192, 4.500000000000000888 ) ) ;
#1606 = CARTESIAN_POINT ( 'NONE',  ( 2.493201789345270480, -65.55452850542926058, -1.934965279058294518 ) ) ;
#1607 = CARTESIAN_POINT ( 'NONE',  ( -6.686770931921503625, -90.60452850542925773, -2.072711028461647675 ) ) ;
#1608 = AXIS2_PLACEMENT_3D ( 'NONE', #7607, #1011, #5115 ) ;
#1609 = ADVANCED_FACE ( 'NONE', ( #1252 ), #3947, .F. ) ;
#1610 = VECTOR ( 'NONE', #6829, 1000.000000000000000 ) ;
#1611 = CARTESIAN_POINT ( 'NONE',  ( 4.191402346623078756, -76.69547149457073942, -5.607243785695398941 ) ) ;
#1612 = DIRECTION ( 'NONE',  ( 0.000000000000000000, -1.000000000000000000, -2.168404344971010347E-16 ) ) ;
#1613 = SHAPE_REPRESENTATION ( 'pin', ( #2840 ), #2157 ) ;
#1614 = DIRECTION ( 'NONE',  ( -0.000000000000000000, -0.000000000000000000, 1.000000000000000000 ) ) ;
#1615 = CARTESIAN_POINT ( 'NONE',  ( -0.8796985632578778747, -88.35452850542924352, 3.030887037049973198 ) ) ;
#1616 = ORIENTED_EDGE ( 'NONE', *, *, #6025, .T. ) ;
#1617 = EDGE_CURVE ( 'NONE', #3327, #7988, #5044, .T. ) ;
#1618 = DIRECTION ( 'NONE',  ( 0.9662349396012460678, 0.2576626505603330508, -0.000000000000000000 ) ) ;
#1619 = CARTESIAN_POINT ( 'NONE',  ( 4.312004677471074743, -67.95452850542922363, 3.009306630940844496 ) ) ;
#1620 = CARTESIAN_POINT ( 'NONE',  ( 4.191402346623078756, -79.69547149457075363, -5.607243785695398941 ) ) ;
#1621 =( NAMED_UNIT ( * ) SI_UNIT ( $, .STERADIAN. ) SOLID_ANGLE_UNIT ( ) );
#1622 = ORIENTED_EDGE ( 'NONE', *, *, #3574, .F. ) ;
#1623 = VECTOR ( 'NONE', #1650, 1000.000000000000000 ) ;
#1624 = CARTESIAN_POINT ( 'NONE',  ( 1.529537955723795140, -72.64547149457074227, 5.030887037049945221 ) ) ;
#1625 = CARTESIAN_POINT ( 'NONE',  ( 5.257311121191341918, -73.24547149457072237, 0.09995255151718437925 ) ) ;
#1626 = CARTESIAN_POINT ( 'NONE',  ( 1.529537955723689002, -65.85452850542924352, -5.030887037049978971 ) ) ;
#1627 = DIRECTION ( 'NONE',  ( -1.261617073437677752E-16, 1.000000000000000000, 0.000000000000000000 ) ) ;
#1628 =( GEOMETRIC_REPRESENTATION_CONTEXT ( 3 ) GLOBAL_UNCERTAINTY_ASSIGNED_CONTEXT ( ( #4856 ) ) GLOBAL_UNIT_ASSIGNED_CONTEXT ( ( #2005, #6383, #3771 ) ) REPRESENTATION_CONTEXT ( 'NONE', 'WORKASPACE' ) );
#1629 = CARTESIAN_POINT ( 'NONE',  ( 4.194503406049401306, -72.94547149457073942, 3.171033256558012159 ) ) ;
#1630 = CARTESIAN_POINT ( 'NONE',  ( 50.00000000000000000, -9.999999999999991118, -10.50000000000000888 ) ) ;
#1631 = CARTESIAN_POINT ( 'NONE',  ( -0.09506052544086367184, -57.00452850542925631, -6.999999999999997335 ) ) ;
#1632 = EDGE_LOOP ( 'NONE', ( #7359, #4290, #4858, #4408, #7822, #4478, #3099, #1119, #7706, #6680, #5713, #6083, #5517, #2025 ) ) ;
#1633 = DIRECTION ( 'NONE',  ( 0.000000000000000000, 0.7071067811865507924, -0.7071067811865441310 ) ) ;
#1634 = EDGE_LOOP ( 'NONE', ( #8213, #7096, #1511, #918, #7592 ) ) ;
#1635 = DIRECTION ( 'NONE',  ( 0.000000000000000000, -1.000000000000000000, -1.734723475976807094E-16 ) ) ;
#1636 = CARTESIAN_POINT ( 'NONE',  ( 0.09506052544086197875, -91.50452850542924921, 4.999999999999997335 ) ) ;
#1637 = CARTESIAN_POINT ( 'NONE',  ( -0.09506052544084034328, -75.00452850542924921, -4.999999999999997335 ) ) ;
#1638 = ORIENTED_EDGE ( 'NONE', *, *, #931, .F. ) ;
#1639 = CARTESIAN_POINT ( 'NONE',  ( 4.312004677471075631, -67.95452850542923784, 3.009306630940844052 ) ) ;
#1640 = CARTESIAN_POINT ( 'NONE',  ( -1.686450176301616644, -80.29547149457074795, -2.482926158054096000 ) ) ;
#1641 = CARTESIAN_POINT ( 'NONE',  ( -1.719659006605263940, -93.34547149457071669, 4.969112962950051227 ) ) ;
#1642 = CARTESIAN_POINT ( 'NONE',  ( 4.312004677471074743, -67.95452850542922363, 3.009306630940844496 ) ) ;
#1643 = CARTESIAN_POINT ( 'NONE',  ( -2.369498399071205963, -87.15452850542926910, -6.969112962950009482 ) ) ;
#1644 = CARTESIAN_POINT ( 'NONE',  ( 1.840261337453268586, -58.80452850542926058, 2.371175808195547852 ) ) ;
#1645 = APPLICATION_PROTOCOL_DEFINITION ( 'draft international standard', 'automotive_design', 1998, #992 ) ;
#1646 = ORIENTED_EDGE ( 'NONE', *, *, #7805, .F. ) ;
#1647 = CARTESIAN_POINT ( 'NONE',  ( 45.00000000000000000, -19.99999999999999645, 4.500000000000000000 ) ) ;
#1648 = PRODUCT_DEFINITION_SHAPE ( 'NONE', 'NONE',  #5608 ) ;
#1649 = VERTEX_POINT ( 'NONE', #573 ) ;
#1650 = DIRECTION ( 'NONE',  ( -1.000000000000000000, 0.000000000000000000, 0.000000000000000000 ) ) ;
#1651 = CARTESIAN_POINT ( 'NONE',  ( 2.610703060766982553, -67.95452850542925205, 1.773238653441072232 ) ) ;
#1652 = CARTESIAN_POINT ( 'NONE',  ( 7.360235569667877620, -76.24547149457073658, 0.09995255151716216091 ) ) ;
#1653 = DIRECTION ( 'NONE',  ( 0.000000000000000000, -1.734723475976807094E-16, 1.000000000000000000 ) ) ;
#1654 = CARTESIAN_POINT ( 'NONE',  ( 45.19324698792023298, -11.84363253063589205, 4.500000000000000888 ) ) ;
#1655 = CARTESIAN_POINT ( 'NONE',  ( -0.09506052544081743105, -90.00452850542926342, -2.999999999999997780 ) ) ;
#1656 = UNCERTAINTY_MEASURE_WITH_UNIT (LENGTH_MEASURE( 1.000000000000000082E-05 ), #4224, 'distance_accuracy_value', 'NONE');
#1657 =( NAMED_UNIT ( * ) SI_UNIT ( $, .STERADIAN. ) SOLID_ANGLE_UNIT ( ) );
#1658 = VERTEX_POINT ( 'NONE', #1294 ) ;
#1659 = EDGE_CURVE ( 'NONE', #250, #417, #4402, .T. ) ;
#1660 = CARTESIAN_POINT ( 'NONE',  ( 50.00000000000000000, -9.999999999999994671, 1.500000000000000666 ) ) ;
#1661 = CARTESIAN_POINT ( 'NONE',  ( 4.725907263620339194, -62.40452850542925489, -1.635492904037697981 ) ) ;
#1662 = CARTESIAN_POINT ( 'NONE',  ( 4.037591185471562483, -75.79547149457074795, 5.718994135553860936 ) ) ;
#1663 = VERTEX_POINT ( 'NONE', #3153 ) ;
#1664 = CARTESIAN_POINT ( 'NONE',  ( -4.312004677470993919, -72.04547149457074795, 3.009306630940933314 ) ) ;
#1665 = CARTESIAN_POINT ( 'NONE',  ( -3.015831842038129817, -69.19547149457073942, 3.989209796945492048 ) ) ;
#1666 = CARTESIAN_POINT ( 'NONE',  ( -3.015831842038215971, -69.30452850542926058, -3.989209796945429432 ) ) ;
#1667 = CARTESIAN_POINT ( 'NONE',  ( 43.45299461620744097, 100.0000000000000000, -7.500000000000000000 ) ) ;
#1668 = ADVANCED_FACE ( 'NONE', ( #5709 ), #2518, .T. ) ;
#1669 = CARTESIAN_POINT ( 'NONE',  ( -0.09506052544073655131, -66.49547149457075079, 4.999999999999997335 ) ) ;
#1670 = SURFACE_STYLE_FILL_AREA ( #2933 ) ;
#1671 = PRESENTATION_LAYER_ASSIGNMENT (  '', '', ( #7728 ) ) ;
#1672 = CARTESIAN_POINT ( 'NONE',  ( 4.725907263620342746, -95.40452850542925489, -1.635492904037697981 ) ) ;
#1673 = VERTEX_POINT ( 'NONE', #4445 ) ;
#1674 = AXIS2_PLACEMENT_3D ( 'NONE', #2882, #3591, #384 ) ;
#1675 = DIRECTION ( 'NONE',  ( 0.9954714945707483498, 0.09506052544079827971, -1.047588144072330487E-14 ) ) ;
#1676 = VECTOR ( 'NONE', #7231, 1000.000000000000000 ) ;
#1677 = ADVANCED_BREP_SHAPE_REPRESENTATION ( '', ( #4428, #2840 ), #1883 ) ;
#1678 = ORIENTED_EDGE ( 'NONE', *, *, #7828, .T. ) ;
#1679 = DIRECTION ( 'NONE',  ( 1.000000000000000000, 0.000000000000000000, 0.000000000000000000 ) ) ;
#1680 = CARTESIAN_POINT ( 'NONE',  ( 1.529537955723691001, -83.85452850542927195, -5.030887037049978971 ) ) ;
#1681 = CARTESIAN_POINT ( 'NONE',  ( 4.784657899331209663, -74.10452850542925773, 1.454677039711774533 ) ) ;
#1682 = CARTESIAN_POINT ( 'NONE',  ( -4.784657899331191899, -60.60452850542925773, -1.454677039711773867 ) ) ;
#1683 = CARTESIAN_POINT ( 'NONE',  ( 0.09506052544077704669, -82.99547149457075079, -2.999999999999997780 ) ) ;
#1684 = CARTESIAN_POINT ( 'NONE',  ( 0.09506052544075753452, -94.99547149457073658, -4.999999999999997335 ) ) ;
#1685 = CARTESIAN_POINT ( 'NONE',  ( 1.719659006605389839, -70.65452850542926910, 4.969112962950016588 ) ) ;
#1686 = CARTESIAN_POINT ( 'NONE',  ( 6.628020296210642037, -89.40452850542926910, -2.253526892787612645 ) ) ;
#1687 = ADVANCED_FACE ( 'NONE', ( #7025 ), #3824, .F. ) ;
#1688 = CARTESIAN_POINT ( 'NONE',  ( -3.154386672714787565, -95.74547149457073658, -0.09995255151720625064 ) ) ;
#1689 = APPLICATION_PROTOCOL_DEFINITION ( 'draft international standard', 'automotive_design', 1998, #7773 ) ;
#1690 = MANIFOLD_SOLID_BREP ( 'Cut-Extrude1', #5315 ) ;
#1691 = ORIENTED_EDGE ( 'NONE', *, *, #2448, .T. ) ;
#1692 = FACE_OUTER_BOUND ( 'NONE', #30, .T. ) ;
#1693 = EDGE_LOOP ( 'NONE', ( #2245, #2702, #999, #617, #3311, #7489, #1691, #2350, #6749 ) ) ;
#1694 = DIRECTION ( 'NONE',  ( 1.000000000000000000, 0.000000000000000000, 0.000000000000000000 ) ) ;
#1695 = CARTESIAN_POINT ( 'NONE',  ( -1.069819614139538855, -72.15452850542922647, -2.969112962950023249 ) ) ;
#1696 = CARTESIAN_POINT ( 'NONE',  ( -2.369498399071057193, -78.34547149457074511, 6.969112962950058332 ) ) ;
#1697 = CARTESIAN_POINT ( 'NONE',  ( -0.09506052544083770650, -96.00452850542926342, -4.999999999999997335 ) ) ;
#1698 =( REPRESENTATION_RELATIONSHIP ('NONE','NONE', #4188, #6502 ) REPRESENTATION_RELATIONSHIP_WITH_TRANSFORMATION ( #4248 )SHAPE_REPRESENTATION_RELATIONSHIP( ) );
#1699 = CARTESIAN_POINT ( 'NONE',  ( -4.194503406049381766, -92.44547149457075363, -3.171033256558012159 ) ) ;
#1700 = CARTESIAN_POINT ( 'NONE',  ( 0.8796985632578994130, -80.85452850542925773, -3.030887037049972310 ) ) ;
#1701 = LINE ( 'NONE', #3757, #1884 ) ;
#1702 = ORIENTED_EDGE ( 'NONE', *, *, #2742, .F. ) ;
#1703 = DIRECTION ( 'NONE',  ( -0.000000000000000000, -0.000000000000000000, 1.000000000000000000 ) ) ;
#1704 = CARTESIAN_POINT ( 'NONE',  ( 0.09506052544085781542, -58.50452850542925631, 4.999999999999997335 ) ) ;
#1705 = CARTESIAN_POINT ( 'NONE',  ( -6.686770931921459216, -68.89547149457074227, 2.072711028461789784 ) ) ;
#1706 = CARTESIAN_POINT ( 'NONE',  ( -65.00000000000000000, -12.00000000000000355, -12.50000000000000178 ) ) ;
#1707 = CARTESIAN_POINT ( 'NONE',  ( 0.09506052544075450916, -70.99547149457075079, -4.999999999999997335 ) ) ;
#1708 = CARTESIAN_POINT ( 'NONE',  ( -4.725907263620355181, -65.59547149457073090, -1.635492904037597617 ) ) ;
#1709 = CARTESIAN_POINT ( 'NONE',  ( -4.194503406049320482, -61.05452850542923926, 3.171033256558100533 ) ) ;
#1710 = CARTESIAN_POINT ( 'NONE',  ( 54.99999999999999289, -30.00000000000000000, -7.500000000000007105 ) ) ;
#1711 = CARTESIAN_POINT ( 'NONE',  ( 1.529537955723793585, -60.64547149457074937, 5.030887037049945221 ) ) ;
#1712 =( NAMED_UNIT ( * ) SI_UNIT ( $, .STERADIAN. ) SOLID_ANGLE_UNIT ( ) );
#1713 = CARTESIAN_POINT ( 'NONE',  ( -4.784657899331188347, -93.60452850542925773, -1.454677039711773867 ) ) ;
#1714 = VERTEX_POINT ( 'NONE', #2229 ) ;
#1715 = CARTESIAN_POINT ( 'NONE',  ( 75.00000000000000000, -19.99999999999999645, -12.50000000000000355 ) ) ;
#1716 = PRODUCT ( 'jaw base', 'jaw base', '', ( #5739 ) ) ;
#1717 = ORIENTED_EDGE ( 'NONE', *, *, #5266, .F. ) ;
#1718 = DIRECTION ( 'NONE',  ( -0.09506052544079829358, 0.9954714945707483498, 0.000000000000000000 ) ) ;
#1719 = CARTESIAN_POINT ( 'NONE',  ( -3.015831842038213750, -87.30452850542926058, -3.989209796945429432 ) ) ;
#1720 = CARTESIAN_POINT ( 'NONE',  ( 4.784657899331179465, -88.39547149457074227, -1.454677039711874009 ) ) ;
#1721 = ADVANCED_FACE ( 'NONE', ( #4785 ), #5294, .F. ) ;
#1722 = CARTESIAN_POINT ( 'NONE',  ( -4.784657899331191011, -66.60452850542924352, -1.454677039711773867 ) ) ;
#1723 = CARTESIAN_POINT ( 'NONE',  ( -0.8796985632579424896, -80.14547149457074227, -3.030887037049952326 ) ) ;
#1724 = CARTESIAN_POINT ( 'NONE',  ( -4.312004677470992142, -84.04547149457074795, 3.009306630940933758 ) ) ;
#1725 = EDGE_CURVE ( 'NONE', #1381, #6629, #3483, .T. ) ;
#1726 = CARTESIAN_POINT ( 'NONE',  ( 1.719659006605389617, -67.65452850542925489, 4.969112962950016588 ) ) ;
#1727 = CARTESIAN_POINT ( 'NONE',  ( 2.369498399071226835, -88.65452850542926910, 6.969112962950009482 ) ) ;
#1728 = VECTOR ( 'NONE', #6153, 1000.000000000000000 ) ;
#1729 = VECTOR ( 'NONE', #7876, 1000.000000000000000 ) ;
#1730 = CARTESIAN_POINT ( 'NONE',  ( -2.493201789345254493, -58.05452850542925347, 1.934965279058294518 ) ) ;
#1731 = ORIENTED_EDGE ( 'NONE', *, *, #2146, .T. ) ;
#1732 = LINE ( 'NONE', #8253, #1601 ) ;
#1733 = ORIENTED_EDGE ( 'NONE', *, *, #2960, .F. ) ;
#1734 = CARTESIAN_POINT ( 'NONE',  ( -3.015831842038213306, -93.30452850542926058, -3.989209796945429432 ) ) ;
#1735 = CARTESIAN_POINT ( 'NONE',  ( -2.493201789345253161, -67.05452850542926058, 1.934965279058294518 ) ) ;
#1736 = CARTESIAN_POINT ( 'NONE',  ( -6.013306294175060351, -75.04547149457074795, 4.245374608440741326 ) ) ;
#1737 = PLANE ( 'NONE',  #3732 ) ;
#1738 = CARTESIAN_POINT ( 'NONE',  ( 3.015831842038150690, -91.69547149457073942, -3.989209796945492048 ) ) ;
#1739 = CARTESIAN_POINT ( 'NONE',  ( 0.8796985632579000791, -86.85452850542924352, -3.030887037049972310 ) ) ;
#1740 =( LENGTH_UNIT ( ) NAMED_UNIT ( * ) SI_UNIT ( .MILLI., .METRE. ) );
#1741 = ORIENTED_EDGE ( 'NONE', *, *, #7805, .T. ) ;
#1742 = FACE_OUTER_BOUND ( 'NONE', #1602, .T. ) ;
#1743 = CARTESIAN_POINT ( 'NONE',  ( -2.823794231030019031, -93.90452850542926910, 1.017458915287783316 ) ) ;
#1744 = VECTOR ( 'NONE', #5258, 1000.000000000000000 ) ;
#1745 = CARTESIAN_POINT ( 'NONE',  ( 7.360235569667877620, -73.24547149457075079, 0.09995255151716216091 ) ) ;
#1746 = CARTESIAN_POINT ( 'NONE',  ( 2.484839419076748879, -97.00000000000000000, -5.444361870252323321 ) ) ;
#1747 = CARTESIAN_POINT ( 'NONE',  ( 4.784657899331176800, -70.39547149457074227, -1.454677039711874009 ) ) ;
#1748 = CARTESIAN_POINT ( 'NONE',  ( -4.312004677470993919, -69.04547149457071953, 3.009306630940933758 ) ) ;
#1749 = CARTESIAN_POINT ( 'NONE',  ( 1.686450176301587334, -92.70452850542926626, -2.482926158054133303 ) ) ;
#1750 = DIRECTION ( 'NONE',  ( 1.000000000000000000, -0.000000000000000000, -0.000000000000000000 ) ) ;
#1751 = PRESENTATION_LAYER_ASSIGNMENT (  '', '', ( #3627 ) ) ;
#1752 = EDGE_CURVE ( 'NONE', #3497, #6231, #2813, .T. ) ;
#1753 = CARTESIAN_POINT ( 'NONE',  ( 1.529537955723689224, -68.85452850542921510, -5.030887037049978971 ) ) ;
#1754 = VECTOR ( 'NONE', #2668, 1000.000000000000000 ) ;
#1755 = CARTESIAN_POINT ( 'NONE',  ( -2.862020680886582014, -65.29547149457073374, -4.100960146803977580 ) ) ;
#1756 = DIRECTION ( 'NONE',  ( 1.000000000000000000, 0.000000000000000000, 0.000000000000000000 ) ) ;
#1757 = VERTEX_POINT ( 'NONE', #4071 ) ;
#1758 = DIRECTION ( 'NONE',  ( -0.5000000000000011102, 0.8660254037844380415, 0.000000000000000000 ) ) ;
#1759 = EDGE_LOOP ( 'NONE', ( #4728, #819, #2885, #1322 ) ) ;
#1760 = CARTESIAN_POINT ( 'NONE',  ( -47.50000000000000711, -54.00000000000000711, 12.50000000000001954 ) ) ;
#1761 = CARTESIAN_POINT ( 'NONE',  ( -4.194503406049316929, -76.05452850542926058, 3.171033256558100533 ) ) ;
#1762 = CARTESIAN_POINT ( 'NONE',  ( 4.312004677471013459, -88.54547149457074795, -3.009306630940933314 ) ) ;
#1763 = CARTESIAN_POINT ( 'NONE',  ( 4.725907263620339194, -59.40452850542926200, -1.635492904037697981 ) ) ;
#1764 = CARTESIAN_POINT ( 'NONE',  ( -1.069819614139474462, -78.34547149457074511, 2.969112962950044121 ) ) ;
#1765 = CARTESIAN_POINT ( 'NONE',  ( -4.037591185471422150, -79.20452850542925205, 5.718994135553947977 ) ) ;
#1766 = CARTESIAN_POINT ( 'NONE',  ( -5.257311121191323267, -83.74547149457075079, -0.09995255151718371311 ) ) ;
#1767 = CARTESIAN_POINT ( 'NONE',  ( 1.529537955723689224, -71.85452850542925773, -5.030887037049978971 ) ) ;
#1768 = CARTESIAN_POINT ( 'NONE',  ( -4.037591185471422150, -79.20452850542925205, 5.718994135553947977 ) ) ;
#1769 = CARTESIAN_POINT ( 'NONE',  ( 1.840261337453221513, -88.69547149457073942, -2.371175808195584267 ) ) ;
#1770 = EDGE_LOOP ( 'NONE', ( #6300, #7373, #537, #2844 ) ) ;
#1771 = CYLINDRICAL_SURFACE ( 'NONE', #790, 1.500000000000001776 ) ;
#1772 = VERTEX_POINT ( 'NONE', #1422 ) ;
#1773 = CARTESIAN_POINT ( 'NONE',  ( -1.719659006605370744, -90.15452850542925489, -4.969112962950015699 ) ) ;
#1774 = CARTESIAN_POINT ( 'NONE',  ( -2.493201789345252717, -73.05452850542926058, 1.934965279058294518 ) ) ;
#1775 = CARTESIAN_POINT ( 'NONE',  ( 4.312004677471079184, -94.95452850542926626, 3.009306630940844496 ) ) ;
#1776 = EDGE_CURVE ( 'NONE', #7622, #8018, #6521, .T. ) ;
#1777 = CARTESIAN_POINT ( 'NONE',  ( 5.895805022753492608, -66.94547149457073942, 4.407101234057782868 ) ) ;
#1778 = CARTESIAN_POINT ( 'NONE',  ( -54.99999999999999289, -100.0000000000000000, 20.00000000000000000 ) ) ;
#1779 = CARTESIAN_POINT ( 'NONE',  ( -4.194503406049382654, -83.44547149457072521, -3.171033256558012159 ) ) ;
#1780 = CARTESIAN_POINT ( 'NONE',  ( 3.154386672714810658, -89.25452850542926342, -0.09995255151727241993 ) ) ;
#1781 = EDGE_CURVE ( 'NONE', #293, #5112, #4033, .T. ) ;
#1782 = ORIENTED_EDGE ( 'NONE', *, *, #937, .T. ) ;
#1783 = CARTESIAN_POINT ( 'NONE',  ( 80.00000000000000000, -25.00000000000000000, 20.00000000000000000 ) ) ;
#1784 = CARTESIAN_POINT ( 'NONE',  ( 1.719659006605388285, -58.65452850542924068, 4.969112962950016588 ) ) ;
#1785 = CARTESIAN_POINT ( 'NONE',  ( -5.895805022753479285, -68.44547149457073942, -4.407101234057782868 ) ) ;
#1786 = SURFACE_STYLE_FILL_AREA ( #471 ) ;
#1787 = CARTESIAN_POINT ( 'NONE',  ( 5.060638198296488532, -96.99999999999998579, 1.908797354467637541 ) ) ;
#1788 = PRODUCT ( 'linear mover', 'linear mover', '', ( #1205 ) ) ;
#1789 = CARTESIAN_POINT ( 'NONE',  ( -2.862020680886582014, -65.29547149457073374, -4.100960146803977580 ) ) ;
#1790 = CARTESIAN_POINT ( 'NONE',  ( -2.862020680886581570, -68.29547149457074795, -4.100960146803977580 ) ) ;
#1791 = CARTESIAN_POINT ( 'NONE',  ( -2.823794231030019031, -90.90452850542926910, 1.017458915287783316 ) ) ;
#1792 = LINE ( 'NONE', #5025, #4464 ) ;
#1793 = EDGE_CURVE ( 'NONE', #5848, #1966, #154, .T. ) ;
#1794 = VECTOR ( 'NONE', #1527, 1000.000000000000000 ) ;
#1795 = CARTESIAN_POINT ( 'NONE',  ( 1.719659006605389839, -70.65452850542926910, 4.969112962950016588 ) ) ;
#1796 = CARTESIAN_POINT ( 'NONE',  ( -4.194503406049384431, -59.44547149457074653, -3.171033256558012159 ) ) ;
#1797 =( LENGTH_UNIT ( ) NAMED_UNIT ( * ) SI_UNIT ( .MILLI., .METRE. ) );
#1798 = VERTEX_POINT ( 'NONE', #7959 ) ;
#1799 = DIRECTION ( 'NONE',  ( -0.000000000000000000, 0.000000000000000000, 1.000000000000000000 ) ) ;
#1800 = VERTEX_POINT ( 'NONE', #828 ) ;
#1801 = CIRCLE ( 'NONE', #1396, 1.499999999999999556 ) ;
#1802 = DIRECTION ( 'NONE',  ( 1.000000000000000000, 1.261617073437677752E-16, 3.501690807976792361E-32 ) ) ;
#1803 = CARTESIAN_POINT ( 'NONE',  ( 4.312004677471075631, -76.95452850542923784, 3.009306630940844496 ) ) ;
#1804 = AXIS2_PLACEMENT_3D ( 'NONE', #5339, #7884, #7325 ) ;
#1805 = CARTESIAN_POINT ( 'NONE',  ( -5.257311121191322378, -89.74547149457070816, -0.09995255151718371311 ) ) ;
#1806 = CARTESIAN_POINT ( 'NONE',  ( -4.784657899331191899, -63.60452850542925063, -1.454677039711773867 ) ) ;
#1807 = CARTESIAN_POINT ( 'NONE',  ( 2.882544866740877065, -73.39547149457074227, -0.8366430509619593447 ) ) ;
#1808 = CARTESIAN_POINT ( 'NONE',  ( -0.09506052544086027178, -84.00452850542926342, -6.999999999999997335 ) ) ;
#1809 = CARTESIAN_POINT ( 'NONE',  ( 4.312004677471013459, -88.54547149457074795, -3.009306630940933314 ) ) ;
#1810 = CARTESIAN_POINT ( 'NONE',  ( -3.015831842038216859, -63.30452850542925347, -3.989209796945429432 ) ) ;
#1811 = CARTESIAN_POINT ( 'NONE',  ( 6.013306294175169597, -73.95452850542925205, 4.245374608440616093 ) ) ;
#1812 = VECTOR ( 'NONE', #4475, 1000.000000000000000 ) ;
#1813 = MECHANICAL_DESIGN_GEOMETRIC_PRESENTATION_REPRESENTATION (  '', ( #6914 ), #1265 ) ;
#1814 = CARTESIAN_POINT ( 'NONE',  ( -1.686450176301615311, -89.29547149457074795, -2.482926158054096000 ) ) ;
#1815 = EDGE_LOOP ( 'NONE', ( #2428, #308, #3461 ) ) ;
#1816 = CARTESIAN_POINT ( 'NONE',  ( 65.00000000000000000, -9.999999999999994671, 10.50000000000000533 ) ) ;
#1817 = CARTESIAN_POINT ( 'NONE',  ( -5.257311121191325931, -59.74547149457072948, -0.09995255151718372699 ) ) ;
#1818 = CIRCLE ( 'NONE', #2086, 1.499999999999994449 ) ;
#1819 = VERTEX_POINT ( 'NONE', #871 ) ;
#1820 = CARTESIAN_POINT ( 'NONE',  ( 1.719659006605392948, -94.65452850542924068, 4.969112962950015699 ) ) ;
#1821 = CARTESIAN_POINT ( 'NONE',  ( 2.493201789345269592, -62.55452850542925347, -1.934965279058294518 ) ) ;
#1822 = CARTESIAN_POINT ( 'NONE',  ( -3.015831842038213306, -93.30452850542926058, -3.989209796945429432 ) ) ;
#1823 = CARTESIAN_POINT ( 'NONE',  ( 2.179377348189628361, -66.64547149457072805, 7.030887037049939003 ) ) ;
#1824 = CARTESIAN_POINT ( 'NONE',  ( -5.257311121191323267, -86.74547149457073658, -0.09995255151718372699 ) ) ;
#1825 = CARTESIAN_POINT ( 'NONE',  ( 3.154386672714808437, -74.25452850542924921, -0.09995255151727241993 ) ) ;
#1826 = CARTESIAN_POINT ( 'NONE',  ( -65.00000000000000000, -7.999999999999996447, 12.49999999999999822 ) ) ;
#1827 = ORIENTED_EDGE ( 'NONE', *, *, #6199, .F. ) ;
#1828 = DIRECTION ( 'NONE',  ( 0.000000000000000000, 0.000000000000000000, 1.000000000000000000 ) ) ;
#1829 = CARTESIAN_POINT ( 'NONE',  ( 1.840261337453273249, -94.80452850542926058, 2.371175808195547852 ) ) ;
#1830 = CARTESIAN_POINT ( 'NONE',  ( -2.369498399071058081, -69.34547149457073090, 6.969112962950058332 ) ) ;
#1831 = PRESENTATION_STYLE_ASSIGNMENT (( #3875 ) ) ;
#1832 = MANIFOLD_SOLID_BREP ( 'Cut-Extrude3', #1963 ) ;
#1833 = DIRECTION ( 'NONE',  ( 1.000000000000000000, 0.000000000000000000, 0.000000000000000000 ) ) ;
#1834 = CARTESIAN_POINT ( 'NONE',  ( -1.529537955723778930, -62.14547149457074937, -5.030887037049945221 ) ) ;
#1835 = CARTESIAN_POINT ( 'NONE',  ( -1.719659006605267937, -60.34547149457073090, 4.969112962950051227 ) ) ;
#1836 = CARTESIAN_POINT ( 'NONE',  ( -0.09506052544084224454, -60.00452850542925631, -4.999999999999997335 ) ) ;
#1837 = ADVANCED_FACE ( 'NONE', ( #7446 ), #2184, .T. ) ;
#1838 = LINE ( 'NONE', #4470, #1924 ) ;
#1839 = CARTESIAN_POINT ( 'NONE',  ( -4.194503406049320482, -64.05452850542926058, 3.171033256558100533 ) ) ;
#1840 = CARTESIAN_POINT ( 'NONE',  ( 4.784657899331175912, -61.39547149457074227, -1.454677039711874009 ) ) ;
#1841 = VERTEX_POINT ( 'NONE', #997 ) ;
#1842 = LINE ( 'NONE', #7145, #3688 ) ;
#1843 = DIRECTION ( 'NONE',  ( 1.000000000000000000, 0.000000000000000000, 0.000000000000000000 ) ) ;
#1844 = ORIENTED_EDGE ( 'NONE', *, *, #4696, .T. ) ;
#1845 = CARTESIAN_POINT ( 'NONE',  ( 47.50000000000002132, 47.23441352194253540, 12.50000000000001954 ) ) ;
#1846 = CARTESIAN_POINT ( 'NONE',  ( 4.784657899331209663, -77.10452850542925773, 1.454677039711774533 ) ) ;
#1847 = CARTESIAN_POINT ( 'NONE',  ( 3.015831842038150246, -88.69547149457073942, -3.989209796945492048 ) ) ;
#1848 = CARTESIAN_POINT ( 'NONE',  ( 4.312004677471074743, -58.95452850542925205, 3.009306630940844052 ) ) ;
#1849 = CARTESIAN_POINT ( 'NONE',  ( 0.09506052544077592259, -73.99547149457075079, -2.999999999999997780 ) ) ;
#1850 = CARTESIAN_POINT ( 'NONE',  ( -4.191402346623178232, -81.30452850542926058, -5.607243785695311900 ) ) ;
#1851 = CARTESIAN_POINT ( 'NONE',  ( 0.09506052544075677124, -88.99547149457073658, -4.999999999999997335 ) ) ;
#1852 = DIRECTION ( 'NONE',  ( -0.000000000000000000, 1.000000000000000000, 2.775557561562891351E-16 ) ) ;
#1853 = CARTESIAN_POINT ( 'NONE',  ( 0.09506052544088175460, -79.50452850542926342, 6.999999999999997335 ) ) ;
#1854 = CARTESIAN_POINT ( 'NONE',  ( -2.493201789345289132, -89.44547149457073942, -1.934965279058240561 ) ) ;
#1855 = EDGE_CURVE ( 'NONE', #6384, #1139, #4766, .T. ) ;
#1856 = ORIENTED_EDGE ( 'NONE', *, *, #1548, .F. ) ;
#1857 = DIRECTION ( 'NONE',  ( 1.000000000000000000, 0.000000000000000000, 0.000000000000000000 ) ) ;
#1858 = CARTESIAN_POINT ( 'NONE',  ( -4.784657899331160813, -59.89547149457074227, 1.454677039711874675 ) ) ;
#1859 = PRODUCT_DEFINITION_SHAPE ( 'NONE', 'NONE',  #6847 ) ;
#1860 = ORIENTED_EDGE ( 'NONE', *, *, #3440, .F. ) ;
#1861 = CARTESIAN_POINT ( 'NONE',  ( 3.015831842038236399, -94.80452850542924637, 3.989209796945429432 ) ) ;
#1862 = CARTESIAN_POINT ( 'NONE',  ( -3.154386672714792006, -60.75452850542924921, 0.09995255151727280851 ) ) ;
#1863 = AXIS2_PLACEMENT_3D ( 'NONE', #2604, #5880, #109 ) ;
#1864 = CARTESIAN_POINT ( 'NONE',  ( -0.09506052544086329714, -60.00452850542925631, -6.999999999999997335 ) ) ;
#1865 = CARTESIAN_POINT ( 'NONE',  ( 4.191402346623077868, -67.69547149457073942, -5.607243785695398941 ) ) ;
#1866 = CARTESIAN_POINT ( 'NONE',  ( 3.015831842038149802, -85.69547149457073942, -3.989209796945492048 ) ) ;
#1867 = CARTESIAN_POINT ( 'NONE',  ( 2.493201789345271369, -74.55452850542926058, -1.934965279058294518 ) ) ;
#1868 = EDGE_CURVE ( 'NONE', #210, #8159, #4313, .T. ) ;
#1869 = DIRECTION ( 'NONE',  ( 0.000000000000000000, 0.000000000000000000, 1.000000000000000000 ) ) ;
#1870 = ADVANCED_FACE ( 'NONE', ( #2353, #3017 ), #481, .T. ) ;
#1871 = CARTESIAN_POINT ( 'NONE',  ( 1.069819614139558617, -88.65452850542926910, 2.969112962950023249 ) ) ;
#1872 = CARTESIAN_POINT ( 'NONE',  ( -7.360235569667860744, -62.74547149457073658, -0.09995255151716124498 ) ) ;
#1873 = CARTESIAN_POINT ( 'NONE',  ( 2.012110789770938712, -97.00000000000001421, -5.644421105825153440 ) ) ;
#1874 = CARTESIAN_POINT ( 'NONE',  ( 4.725907263620371168, -61.09547149457074511, 1.635492904037598283 ) ) ;
#1875 = CARTESIAN_POINT ( 'NONE',  ( -6.686770931921456551, -95.89547149457075648, 2.072711028461789784 ) ) ;
#1876 = CARTESIAN_POINT ( 'NONE',  ( 0.09506052544084107880, -94.50452850542926342, 2.999999999999997780 ) ) ;
#1877 = FACE_OUTER_BOUND ( 'NONE', #6061, .T. ) ;
#1878 = VECTOR ( 'NONE', #1091, 1000.000000000000000 ) ;
#1879 = CARTESIAN_POINT ( 'NONE',  ( -2.862020680886495416, -70.20452850542925205, 4.100960146804039752 ) ) ;
#1880 = EDGE_CURVE ( 'NONE', #5175, #2862, #2389, .T. ) ;
#1881 = CARTESIAN_POINT ( 'NONE',  ( -6.628020296210665130, -92.59547149457074511, -2.253526892787471869 ) ) ;
#1882 = ORIENTED_EDGE ( 'NONE', *, *, #4850, .T. ) ;
#1883 =( GEOMETRIC_REPRESENTATION_CONTEXT ( 3 ) GLOBAL_UNCERTAINTY_ASSIGNED_CONTEXT ( ( #2253 ) ) GLOBAL_UNIT_ASSIGNED_CONTEXT ( ( #7434, #6205, #429 ) ) REPRESENTATION_CONTEXT ( 'NONE', 'WORKASPACE' ) );
#1884 = VECTOR ( 'NONE', #8224, 1000.000000000000000 ) ;
#1885 = CARTESIAN_POINT ( 'NONE',  ( 54.99999999999999289, 50.00000000000000000, 7.500000000000000000 ) ) ;
#1886 = VECTOR ( 'NONE', #3859, 1000.000000000000000 ) ;
#1887 = ORIENTED_EDGE ( 'NONE', *, *, #4926, .T. ) ;
#1888 = CARTESIAN_POINT ( 'NONE',  ( 65.00000000000000000, -12.00000000000000355, -12.50000000000000178 ) ) ;
#1889 = CARTESIAN_POINT ( 'NONE',  ( -4.784657899331190123, -81.60452850542925773, -1.454677039711773867 ) ) ;
#1890 = CARTESIAN_POINT ( 'NONE',  ( 2.862020680886600221, -84.79547149457074795, 4.100960146803977580 ) ) ;
#1891 = CARTESIAN_POINT ( 'NONE',  ( 3.924576421043429963, -96.99999999999988631, -1.488513849420440627 ) ) ;
#1892 = CARTESIAN_POINT ( 'NONE',  ( -1.686450176301617976, -71.29547149457074795, -2.482926158054096000 ) ) ;
#1893 = CARTESIAN_POINT ( 'NONE',  ( -6.686770931921506289, -78.60452850542927195, -2.072711028461647675 ) ) ;
#1894 = CARTESIAN_POINT ( 'NONE',  ( -2.862020680886578905, -92.29547149457074795, -4.100960146803977580 ) ) ;
#1895 = DIRECTION ( 'NONE',  ( 1.000000000000000000, 0.000000000000000000, 0.000000000000000000 ) ) ;
#1896 =( GEOMETRIC_REPRESENTATION_CONTEXT ( 3 ) GLOBAL_UNCERTAINTY_ASSIGNED_CONTEXT ( ( #896 ) ) GLOBAL_UNIT_ASSIGNED_CONTEXT ( ( #4515, #640, #7095 ) ) REPRESENTATION_CONTEXT ( 'NONE', 'WORKASPACE' ) );
#1897 = CARTESIAN_POINT ( 'NONE',  ( 4.037591185471443467, -80.70452850542925205, -5.718994135553947977 ) ) ;
#1898 = CARTESIAN_POINT ( 'NONE',  ( -0.09506052544075518917, -87.49547149457075079, 2.999999999999997780 ) ) ;
#1899 = ORIENTED_EDGE ( 'NONE', *, *, #4820, .F. ) ;
#1900 = CARTESIAN_POINT ( 'NONE',  ( 3.943604702053941724E-15, -27.99999999999999645, -2.499999999999999112 ) ) ;
#1901 = CARTESIAN_POINT ( 'NONE',  ( 50.00000000000000000, -7.999999999999992895, -12.50000000000000178 ) ) ;
#1902 = VERTEX_POINT ( 'NONE', #6846 ) ;
#1903 = CARTESIAN_POINT ( 'NONE',  ( -4.725907263620320542, -81.90452850542925489, 1.635492904037698647 ) ) ;
#1904 = CARTESIAN_POINT ( 'NONE',  ( 2.610703060766947914, -97.54547149457074795, -1.773238653441125523 ) ) ;
#1905 = CARTESIAN_POINT ( 'NONE',  ( 4.194503406049339134, -92.55452850542924637, -3.171033256558100089 ) ) ;
#1906 = CARTESIAN_POINT ( 'NONE',  ( 6.013306294175077227, -73.54547149457074795, -4.245374608440741326 ) ) ;
#1907 = CARTESIAN_POINT ( 'NONE',  ( 4.312004677471013459, -85.54547149457073374, -3.009306630940932425 ) ) ;
#1908 = CARTESIAN_POINT ( 'NONE',  ( -1.686450176301566017, -76.20452850542925205, 2.482926158054133303 ) ) ;
#1909 = CARTESIAN_POINT ( 'NONE',  ( -80.00100000000001899, -93.00000000000004263, 6.123233995736772199E-16 ) ) ;
#1910 = DIRECTION ( 'NONE',  ( -0.000000000000000000, 0.7071067811865442421, 0.7071067811865509034 ) ) ;
#1911 = CARTESIAN_POINT ( 'NONE',  ( 1.840261337453271917, -85.80452850542926058, 2.371175808195547852 ) ) ;
#1912 = CARTESIAN_POINT ( 'NONE',  ( 2.369498399071075845, -64.84547149457071669, -6.969112962950057444 ) ) ;
#1913 = ADVANCED_FACE ( 'NONE', ( #4275 ), #2936, .F. ) ;
#1914 = PLANE ( 'NONE',  #6045 ) ;
#1915 = CARTESIAN_POINT ( 'NONE',  ( -5.257311121191325043, -62.74547149457074369, -0.09995255151718372699 ) ) ;
#1916 = CARTESIAN_POINT ( 'NONE',  ( 5.895805022753496161, -93.94547149457073942, 4.407101234057782868 ) ) ;
#1917 = DIRECTION ( 'NONE',  ( 1.000000000000000000, 2.775557561562892337E-16, -0.000000000000000000 ) ) ;
#1918 = LINE ( 'NONE', #514, #2199 ) ;
#1919 = EDGE_CURVE ( 'NONE', #5503, #914, #7407, .T. ) ;
#1920 = CARTESIAN_POINT ( 'NONE',  ( 4.725907263620340082, -68.40452850542925489, -1.635492904037697981 ) ) ;
#1921 = CARTESIAN_POINT ( 'NONE',  ( -2.179377348189609265, -89.14547149457072805, -7.030887037049939003 ) ) ;
#1922 = VERTEX_POINT ( 'NONE', #3564 ) ;
#1923 = CARTESIAN_POINT ( 'NONE',  ( 4.336808689942017736E-15, -22.00000000000000000, -2.499999999999999112 ) ) ;
#1924 = VECTOR ( 'NONE', #8233, 1000.000000000000000 ) ;
#1925 = ORIENTED_EDGE ( 'NONE', *, *, #1060, .T. ) ;
#1926 = CARTESIAN_POINT ( 'NONE',  ( -0.9662349396012467340, -27.25766265056033433, 2.500000000000000888 ) ) ;
#1927 = CARTESIAN_POINT ( 'NONE',  ( -5.257311121191324155, -78.75452850542924921, 0.09995255151729526277 ) ) ;
#1928 = CARTESIAN_POINT ( 'NONE',  ( -3.015831842038129373, -75.19547149457073942, 3.989209796945492048 ) ) ;
#1929 = CARTESIAN_POINT ( 'NONE',  ( 4.336808689942017736E-15, -22.00000000000000000, 2.500000000000000888 ) ) ;
#1930 = CARTESIAN_POINT ( 'NONE',  ( -2.493201789345292241, -68.44547149457073942, -1.934965279058240561 ) ) ;
#1931 = CARTESIAN_POINT ( 'NONE',  ( -7.360235569667858968, -75.75452850542926342, 0.09995255151731782806 ) ) ;
#1932 = CARTESIAN_POINT ( 'NONE',  ( 5.257311121191341918, -76.24547149457073658, 0.09995255151718437925 ) ) ;
#1933 = SHAPE_REPRESENTATION ( 'arm', ( #2840 ), #5779 ) ;
#1934 = CARTESIAN_POINT ( 'NONE',  ( -4.725907263620324095, -57.90452850542925489, 1.635492904037698647 ) ) ;
#1935 = CARTESIAN_POINT ( 'NONE',  ( 55.00000000000000000, -25.00000000000002132, 20.00000000000000000 ) ) ;
#1936 = CARTESIAN_POINT ( 'NONE',  ( 2.179377348189481811, -77.85452850542925773, -7.030887037049986077 ) ) ;
#1937 = CARTESIAN_POINT ( 'NONE',  ( -2.823794231030039459, -83.59547149457075932, -1.017458915287723364 ) ) ;
#1938 = AXIS2_PLACEMENT_3D ( 'NONE', #2859, #915, #282 ) ;
#1939 = ORIENTED_EDGE ( 'NONE', *, *, #7378, .F. ) ;
#1940 = DIRECTION ( 'NONE',  ( 0.000000000000000000, 0.000000000000000000, -1.000000000000000000 ) ) ;
#1941 = CARTESIAN_POINT ( 'NONE',  ( 65.00000000000000000, -7.999999999999992895, -12.50000000000000178 ) ) ;
#1942 = CARTESIAN_POINT ( 'NONE',  ( -5.257311121191323267, -84.75452850542923500, 0.09995255151729526277 ) ) ;
#1943 = ORIENTED_EDGE ( 'NONE', *, *, #2448, .F. ) ;
#1944 = CARTESIAN_POINT ( 'NONE',  ( 4.784657899331209663, -77.10452850542925773, 1.454677039711774533 ) ) ;
#1945 = CARTESIAN_POINT ( 'NONE',  ( 0.8796985632578967484, -59.85452850542925773, -3.030887037049972310 ) ) ;
#1946 = EDGE_CURVE ( 'NONE', #1594, #540, #729, .T. ) ;
#1947 = CARTESIAN_POINT ( 'NONE',  ( -4.312004677471055203, -93.45452850542922363, -3.009306630940844052 ) ) ;
#1948 = AXIS2_PLACEMENT_3D ( 'NONE', #4723, #2211, #6078 ) ;
#1949 = AXIS2_PLACEMENT_3D ( 'NONE', #4301, #7678, #4461 ) ;
#1950 = CARTESIAN_POINT ( 'NONE',  ( -0.09506052544071530441, -66.49547149457075079, 6.999999999999997335 ) ) ;
#1951 = CARTESIAN_POINT ( 'NONE',  ( 1.529537955723797360, -90.64547149457075648, 5.030887037049945221 ) ) ;
#1952 = CARTESIAN_POINT ( 'NONE',  ( -3.154386672714790674, -72.75452850542926342, 0.09995255151727280851 ) ) ;
#1953 = AXIS2_PLACEMENT_3D ( 'NONE', #1496, #776, #4106 ) ;
#1954 = FACE_BOUND ( 'NONE', #3515, .T. ) ;
#1955 = CARTESIAN_POINT ( 'NONE',  ( 50.00000000000000000, -9.999999999999994671, 0.000000000000000000 ) ) ;
#1956 = CARTESIAN_POINT ( 'NONE',  ( -2.610703060766963901, -84.45452850542925205, -1.773238653441072232 ) ) ;
#1957 = CARTESIAN_POINT ( 'NONE',  ( 0.09506052544073274879, -64.99547149457075079, -6.999999999999997335 ) ) ;
#1958 = LINE ( 'NONE', #4465, #4286 ) ;
#1959 = CARTESIAN_POINT ( 'NONE',  ( 1.529537955723794473, -66.64547149457072805, 5.030887037049945221 ) ) ;
#1960 = CARTESIAN_POINT ( 'NONE',  ( 4.312004677471010794, -61.54547149457073374, -3.009306630940933314 ) ) ;
#1961 = FACE_OUTER_BOUND ( 'NONE', #7933, .T. ) ;
#1962 = DIRECTION ( 'NONE',  ( -1.000000000000000000, -1.261617073437677752E-16, -3.501690807976792361E-32 ) ) ;
#1963 = CLOSED_SHELL ( 'NONE', ( #3411, #1032, #3271, #2345, #4211, #4487, #898, #6158, #3057, #5097, #7630, #779, #7010, #1164, #5712, #1460, #2041, #6132, #5943, #1687, #4380, #1514, #6128, #7098, #2710, #769, #5212, #5379, #94, #8306, #3727, #7921, #1668, #1609, #3609, #5284, #7576, #1204, #6288, #950, #1118 ) ) ;
#1964 = CARTESIAN_POINT ( 'NONE',  ( -4.784657899331191899, -60.60452850542925773, -1.454677039711773867 ) ) ;
#1965 = CARTESIAN_POINT ( 'NONE',  ( -2.369498399071055417, -90.34547149457073090, 6.969112962950058332 ) ) ;
#1966 = VERTEX_POINT ( 'NONE', #6133 ) ;
#1967 = CARTESIAN_POINT ( 'NONE',  ( 1.529537955723689890, -74.85452850542925773, -5.030887037049978971 ) ) ;
#1968 = CARTESIAN_POINT ( 'NONE',  ( 47.49999999999998579, -93.00000000000000000, 6.123233995736772199E-16 ) ) ;
#1969 = CONTEXT_DEPENDENT_SHAPE_REPRESENTATION ( #5714, #3632 ) ;
#1970 = DIRECTION ( 'NONE',  ( 0.000000000000000000, -0.000000000000000000, 1.000000000000000000 ) ) ;
#1971 = CARTESIAN_POINT ( 'NONE',  ( -1.719659006605264384, -84.34547149457071669, 4.969112962950051227 ) ) ;
#1972 = CARTESIAN_POINT ( 'NONE',  ( 4.282105902239295325, -96.99999999999998579, 2.536915707574844525 ) ) ;
#1973 = CARTESIAN_POINT ( 'NONE',  ( 2.823794231030058555, -67.09547149457073090, 1.017458915287723809 ) ) ;
#1974 = CARTESIAN_POINT ( 'NONE',  ( 6.013306294175168709, -70.95452850542925205, 4.245374608440616093 ) ) ;
#1975 = LINE ( 'NONE', #7195, #7322 ) ;
#1976 = CARTESIAN_POINT ( 'NONE',  ( 0.09506052544075600796, -82.99547149457075079, -4.999999999999997335 ) ) ;
#1977 = CARTESIAN_POINT ( 'NONE',  ( 5.257311121191341918, -62.25452850542924921, -0.09995255151729465215 ) ) ;
#1978 = CARTESIAN_POINT ( 'NONE',  ( 3.015831842038235955, -91.80452850542926058, 3.989209796945429432 ) ) ;
#1979 = CARTESIAN_POINT ( 'NONE',  ( -7.360235569667858968, -72.75452850542926342, 0.09995255151731782806 ) ) ;
#1980 = CARTESIAN_POINT ( 'NONE',  ( 2.882544866740877509, -76.39547149457074227, -0.8366430509619593447 ) ) ;
#1981 = EDGE_CURVE ( 'NONE', #6079, #943, #357, .T. ) ;
#1982 = ORIENTED_EDGE ( 'NONE', *, *, #7035, .T. ) ;
#1983 = DIRECTION ( 'NONE',  ( 0.000000000000000000, -1.000000000000000000, -1.734723475976807094E-16 ) ) ;
#1984 = LINE ( 'NONE', #3707, #5974 ) ;
#1985 = CARTESIAN_POINT ( 'NONE',  ( 1.529537955723691889, -86.85452850542921510, -5.030887037049978971 ) ) ;
#1986 = ORIENTED_EDGE ( 'NONE', *, *, #3601, .F. ) ;
#1987 = CARTESIAN_POINT ( 'NONE',  ( -4.194503406049316929, -79.05452850542923215, 3.171033256558101865 ) ) ;
#1988 = CARTESIAN_POINT ( 'NONE',  ( -2.493201789345254493, -58.05452850542925347, 1.934965279058294518 ) ) ;
#1989 = SHAPE_REPRESENTATION ( 'linear mover', ( #2840 ), #6190 ) ;
#1990 = CARTESIAN_POINT ( 'NONE',  ( -4.312004677471056979, -84.45452850542922363, -3.009306630940844052 ) ) ;
#1991 = CARTESIAN_POINT ( 'NONE',  ( 5.895805022753407343, -92.55452850542926058, -4.407101234057908989 ) ) ;
#1992 = CARTESIAN_POINT ( 'NONE',  ( -4.725907263620353405, -80.59547149457074511, -1.635492904037597617 ) ) ;
#1993 = CARTESIAN_POINT ( 'NONE',  ( -0.8796985632578793179, -76.35452850542924352, 3.030887037049973198 ) ) ;
#1994 = DIRECTION ( 'NONE',  ( 0.000000000000000000, 0.000000000000000000, 1.000000000000000000 ) ) ;
#1995 = CARTESIAN_POINT ( 'NONE',  ( 47.49999999999999289, -20.00000000000000355, 12.49999999999999112 ) ) ;
#1996 = CARTESIAN_POINT ( 'NONE',  ( -2.823794231030019919, -84.90452850542926910, 1.017458915287783316 ) ) ;
#1997 = CARTESIAN_POINT ( 'NONE',  ( -4.037591185471547384, -59.29547149457074084, -5.718994135553860936 ) ) ;
#1998 = LINE ( 'NONE', #6413, #1328 ) ;
#1999 = CARTESIAN_POINT ( 'NONE',  ( -4.194503406049316041, -79.05452850542921794, 3.171033256558100533 ) ) ;
#2000 = CARTESIAN_POINT ( 'NONE',  ( 6.686770931921479644, -94.39547149457074227, -2.072711028461788896 ) ) ;
#2001 = CARTESIAN_POINT ( 'NONE',  ( 45.00000000000000000, -14.99999999999999467, -12.50000000000000178 ) ) ;
#2002 = DIRECTION ( 'NONE',  ( 1.000000000000000000, 0.000000000000000000, 0.000000000000000000 ) ) ;
#2003 = CARTESIAN_POINT ( 'NONE',  ( 1.719659006605388285, -58.65452850542924068, 4.969112962950016588 ) ) ;
#2004 = CARTESIAN_POINT ( 'NONE',  ( 4.037591185471564259, -90.79547149457074795, 5.718994135553860936 ) ) ;
#2005 =( LENGTH_UNIT ( ) NAMED_UNIT ( * ) SI_UNIT ( .MILLI., .METRE. ) );
#2006 = ORIENTED_EDGE ( 'NONE', *, *, #158, .F. ) ;
#2007 = CARTESIAN_POINT ( 'NONE',  ( -1.719659006605371854, -78.15452850542925489, -4.969112962950016588 ) ) ;
#2008 = CARTESIAN_POINT ( 'NONE',  ( 45.00000000000000000, -14.99999999999999467, 4.500000000000000888 ) ) ;
#2009 = VECTOR ( 'NONE', #6944, 1000.000000000000000 ) ;
#2010 = DIRECTION ( 'NONE',  ( -1.000000000000000000, 0.000000000000000000, 0.000000000000000000 ) ) ;
#2011 = CARTESIAN_POINT ( 'NONE',  ( -5.257311121191323267, -83.74547149457075079, -0.09995255151718371311 ) ) ;
#2012 = LINE ( 'NONE', #3190, #2032 ) ;
#2013 = CARTESIAN_POINT ( 'NONE',  ( 1.840261337453218626, -61.69547149457074653, -2.371175808195584267 ) ) ;
#2014 = AXIS2_PLACEMENT_3D ( 'NONE', #8099, #2487, #4289 ) ;
#2015 = CARTESIAN_POINT ( 'NONE',  ( -2.179377348189461827, -73.35452850542924352, 7.030887037049988741 ) ) ;
#2016 = CARTESIAN_POINT ( 'NONE',  ( 45.00000000000000000, -14.99999999999999467, 2.500000000000000888 ) ) ;
#2017 = PRODUCT_DEFINITION ( 'UNKNOWN', '', #4690, #4178 ) ;
#2018 = CARTESIAN_POINT ( 'NONE',  ( 1.719659006605285922, -76.84547149457073090, -4.969112962950050338 ) ) ;
#2019 = APPLICATION_CONTEXT ( 'automotive_design' ) ;
#2020 = CARTESIAN_POINT ( 'NONE',  ( 0.09506052544085819012, -61.50452850542925631, 4.999999999999997335 ) ) ;
#2021 = CARTESIAN_POINT ( 'NONE',  ( -2.862020680886492752, -88.20452850542925205, 4.100960146804039752 ) ) ;
#2022 = CARTESIAN_POINT ( 'NONE',  ( 2.179377348189480923, -68.85452850542924352, -7.030887037049986077 ) ) ;
#2023 = CARTESIAN_POINT ( 'NONE',  ( 1.686450176301585335, -77.70452850542925205, -2.482926158054133303 ) ) ;
#2024 = CARTESIAN_POINT ( 'NONE',  ( 2.882544866740877954, -79.39547149457074227, -0.8366430509619593447 ) ) ;
#2025 = ORIENTED_EDGE ( 'NONE', *, *, #6810, .F. ) ;
#2026 = CARTESIAN_POINT ( 'NONE',  ( 45.00000000000000000, -19.99999999999999645, 9.500000000000000000 ) ) ;
#2027 = DIRECTION ( 'NONE',  ( 0.000000000000000000, 0.000000000000000000, 1.000000000000000000 ) ) ;
#2028 = CARTESIAN_POINT ( 'NONE',  ( 0.09506052544086121547, -85.50452850542926342, 4.999999999999997335 ) ) ;
#2029 = EDGE_LOOP ( 'NONE', ( #4288, #7071 ) ) ;
#2030 = CARTESIAN_POINT ( 'NONE',  ( -1.719659006605371854, -81.15452850542924068, -4.969112962950015699 ) ) ;
#2031 = CARTESIAN_POINT ( 'NONE',  ( -1.840261337453198198, -93.19547149457075363, 2.371175808195584267 ) ) ;
#2032 = VECTOR ( 'NONE', #3902, 1000.000000000000000 ) ;
#2033 = DIRECTION ( 'NONE',  ( -1.000000000000000000, 0.000000000000000000, 0.000000000000000000 ) ) ;
#2034 = CARTESIAN_POINT ( 'NONE',  ( 3.015831842038235511, -88.80452850542926058, 3.989209796945429432 ) ) ;
#2035 = EDGE_CURVE ( 'NONE', #8322, #1841, #1117, .T. ) ;
#2036 = CARTESIAN_POINT ( 'NONE',  ( 6.628020296210686446, -64.09547149457071669, 2.253526892787472757 ) ) ;
#2037 = CARTESIAN_POINT ( 'NONE',  ( 1.840261337453269253, -64.80452850542926058, 2.371175808195547852 ) ) ;
#2038 = CARTESIAN_POINT ( 'NONE',  ( 6.123233995736760366E-16, -27.00000000000000000, 2.500000000000000888 ) ) ;
#2039 = FACE_OUTER_BOUND ( 'NONE', #6713, .T. ) ;
#2040 = CARTESIAN_POINT ( 'NONE',  ( -1.686450176301564241, -88.20452850542925205, 2.482926158054133303 ) ) ;
#2041 = ADVANCED_FACE ( 'NONE', ( #5501 ), #3649, .F. ) ;
#2042 = CARTESIAN_POINT ( 'NONE',  ( -6.013306294175061240, -66.04547149457074795, 4.245374608440741326 ) ) ;
#2043 = CARTESIAN_POINT ( 'NONE',  ( 6.123233995736760366E-16, -27.00000000000000000, 5.000000000000000000 ) ) ;
#2044 = CARTESIAN_POINT ( 'NONE',  ( -3.015831842038215083, -75.30452850542926058, -3.989209796945429432 ) ) ;
#2045 = CARTESIAN_POINT ( 'NONE',  ( 4.037591185471564259, -87.79547149457074795, 5.718994135553860936 ) ) ;
#2046 = CARTESIAN_POINT ( 'NONE',  ( -47.50000000000000711, -51.00000000000000711, 12.50000000000001954 ) ) ;
#2047 = LINE ( 'NONE', #2718, #1794 ) ;
#2048 = CARTESIAN_POINT ( 'NONE',  ( -0.09506052544075783983, -66.49547149457075079, 2.999999999999997780 ) ) ;
#2049 = CARTESIAN_POINT ( 'NONE',  ( 6.013306294175080779, -88.54547149457074795, -4.245374608440741326 ) ) ;
#2050 = FILL_AREA_STYLE_COLOUR ( '', #3641 ) ;
#2051 = ORIENTED_EDGE ( 'NONE', *, *, #6707, .F. ) ;
#2052 = CARTESIAN_POINT ( 'NONE',  ( -0.09506052544084073186, -72.00452850542926342, -4.999999999999997335 ) ) ;
#2053 = ADVANCED_FACE ( 'NONE', ( #3691, #4355 ), #6262, .T. ) ;
#2054 = DIRECTION ( 'NONE',  ( 0.000000000000000000, -1.000000000000000000, -2.168404344971010347E-16 ) ) ;
#2055 = LINE ( 'NONE', #4603, #1133 ) ;
#2056 = CARTESIAN_POINT ( 'NONE',  ( -2.862020680886580237, -80.29547149457074795, -4.100960146803977580 ) ) ;
#2057 = CARTESIAN_POINT ( 'NONE',  ( 4.239768230324508558, -96.99999999999998579, 2.450885936931344045 ) ) ;
#2058 = CARTESIAN_POINT ( 'NONE',  ( 2.493201789345308228, -63.94547149457074653, 1.934965279058241006 ) ) ;
#2059 = CARTESIAN_POINT ( 'NONE',  ( -4.191402346623179120, -72.30452850542926058, -5.607243785695311900 ) ) ;
#2060 = CYLINDRICAL_SURFACE ( 'NONE', #452, 1.500000000000001332 ) ;
#2061 = CARTESIAN_POINT ( 'NONE',  ( -1.719659006605265272, -75.34547149457074511, 4.969112962950051227 ) ) ;
#2062 = CARTESIAN_POINT ( 'NONE',  ( -4.312004677471056091, -87.45452850542925205, -3.009306630940844052 ) ) ;
#2063 = CARTESIAN_POINT ( 'NONE',  ( -6.628020296210620721, -72.90452850542925489, 2.253526892787613978 ) ) ;
#2064 = CARTESIAN_POINT ( 'NONE',  ( 0.09506052544077592259, -73.99547149457075079, -2.999999999999997780 ) ) ;
#2065 = ORIENTED_EDGE ( 'NONE', *, *, #991, .T. ) ;
#2066 = DIRECTION ( 'NONE',  ( 0.000000000000000000, -1.000000000000000000, 3.469446951953616161E-16 ) ) ;
#2067 = DIRECTION ( 'NONE',  ( -0.000000000000000000, 1.000000000000000000, 2.775557561562891351E-16 ) ) ;
#2068 = CARTESIAN_POINT ( 'NONE',  ( 4.312004677471078296, -91.95452850542925205, 3.009306630940844496 ) ) ;
#2069 = ORIENTED_EDGE ( 'NONE', *, *, #2485, .T. ) ;
#2070 = CARTESIAN_POINT ( 'NONE',  ( -0.09506052544083998246, -78.00452850542926342, -4.999999999999997335 ) ) ;
#2071 = CARTESIAN_POINT ( 'NONE',  ( 2.882544866740879286, -91.39547149457074227, -0.8366430509619593447 ) ) ;
#2072 = DIRECTION ( 'NONE',  ( 0.000000000000000000, 0.000000000000000000, 1.000000000000000000 ) ) ;
#2073 = CARTESIAN_POINT ( 'NONE',  ( 0.09506052544086084077, -82.50452850542926342, 4.999999999999997335 ) ) ;
#2074 = CARTESIAN_POINT ( 'NONE',  ( -2.179377348189612817, -62.14547149457074937, -7.030887037049939003 ) ) ;
#2075 = CARTESIAN_POINT ( 'NONE',  ( 2.823794231030038571, -62.40452850542925489, -1.017458915287783316 ) ) ;
#2076 = DIRECTION ( 'NONE',  ( 0.5000000000000011102, -0.8660254037844380415, 0.000000000000000000 ) ) ;
#2077 = CARTESIAN_POINT ( 'NONE',  ( 0.7729879516809982087, -29.89870481880373987, 4.500000000000000888 ) ) ;
#2078 = CARTESIAN_POINT ( 'NONE',  ( 0.8796985632578994130, -80.85452850542925773, -3.030887037049972310 ) ) ;
#2079 = CARTESIAN_POINT ( 'NONE',  ( 4.191402346623198660, -88.80452850542926058, 5.607243785695311900 ) ) ;
#2080 = VECTOR ( 'NONE', #1703, 1000.000000000000000 ) ;
#2081 = LINE ( 'NONE', #5814, #3620 ) ;
#2082 = CARTESIAN_POINT ( 'NONE',  ( -0.09506052544071304233, -84.49547149457075079, 6.999999999999997335 ) ) ;
#2083 = LINE ( 'NONE', #4638, #499 ) ;
#2084 = CARTESIAN_POINT ( 'NONE',  ( 55.00000000000002132, -82.99999999999998579, 0.000000000000000000 ) ) ;
#2085 = CARTESIAN_POINT ( 'NONE',  ( 2.823794231030058999, -70.09547149457073090, 1.017458915287723809 ) ) ;
#2086 = AXIS2_PLACEMENT_3D ( 'NONE', #2008, #1283, #2469 ) ;
#2087 = PRESENTATION_STYLE_ASSIGNMENT (( #767 ) ) ;
#2088 = VERTEX_POINT ( 'NONE', #6805 ) ;
#2089 = CARTESIAN_POINT ( 'NONE',  ( 4.725907263620340082, -71.40452850542925489, -1.635492904037697981 ) ) ;
#2090 = CARTESIAN_POINT ( 'NONE',  ( 6.013306294175077227, -76.54547149457074795, -4.245374608440741326 ) ) ;
#2091 = AXIS2_PLACEMENT_3D ( 'NONE', #3056, #4236, #1163 ) ;
#2092 = EDGE_CURVE ( 'NONE', #9, #1819, #8198, .T. ) ;
#2093 = ORIENTED_EDGE ( 'NONE', *, *, #2146, .F. ) ;
#2094 = CARTESIAN_POINT ( 'NONE',  ( 4.784657899331209663, -77.10452850542925773, 1.454677039711774533 ) ) ;
#2095 = CARTESIAN_POINT ( 'NONE',  ( 65.00000000000000000, -12.00000000000000355, -12.50000000000000178 ) ) ;
#2096 = ITEM_DEFINED_TRANSFORMATION ( 'NONE', 'NONE', #6176,  #2840 ) ;
#2097 = DIRECTION ( 'NONE',  ( 0.000000000000000000, 0.000000000000000000, -1.000000000000000000 ) ) ;
#2098 = CARTESIAN_POINT ( 'NONE',  ( -1.529537955723776710, -80.14547149457072805, -5.030887037049945221 ) ) ;
#2099 = CARTESIAN_POINT ( 'NONE',  ( 1.500000000000001998, -26.99999999999998934, -7.000000000000000000 ) ) ;
#2100 = CARTESIAN_POINT ( 'NONE',  ( 4.725907263620375609, -97.09547149457074511, 1.635492904037598283 ) ) ;
#2101 = CARTESIAN_POINT ( 'NONE',  ( -6.013306294175152722, -72.45452850542925205, -4.245374608440613429 ) ) ;
#2102 = CARTESIAN_POINT ( 'NONE',  ( 65.00000000000000000, -7.999999999999996447, 12.49999999999999822 ) ) ;
#2103 = CARTESIAN_POINT ( 'NONE',  ( -4.725907263620353405, -74.59547149457074511, -1.635492904037597617 ) ) ;
#2104 = CARTESIAN_POINT ( 'NONE',  ( -1.529537955723668796, -85.35452850542924352, 5.030887037049979860 ) ) ;
#2105 = CARTESIAN_POINT ( 'NONE',  ( -4.037591185471423039, -73.20452850542925205, 5.718994135553947977 ) ) ;
#2106 = CARTESIAN_POINT ( 'NONE',  ( -2.493201789345290464, -83.44547149457073942, -1.934965279058240561 ) ) ;
#2107 = ORIENTED_EDGE ( 'NONE', *, *, #3963, .F. ) ;
#2108 = LINE ( 'NONE', #5383, #718 ) ;
#2109 = CARTESIAN_POINT ( 'NONE',  ( 1.529537955723692555, -92.85452850542925773, -5.030887037049978971 ) ) ;
#2110 = CARTESIAN_POINT ( 'NONE',  ( 2.862020680886514956, -83.70452850542925205, -4.100960146804039752 ) ) ;
#2111 = ORIENTED_EDGE ( 'NONE', *, *, #6840, .F. ) ;
#2112 = CARTESIAN_POINT ( 'NONE',  ( -5.257311121191325043, -75.75452850542923500, 0.09995255151729529053 ) ) ;
#2113 = CARTESIAN_POINT ( 'NONE',  ( 1.069819614139496000, -88.84547149457073090, -2.969112962950042789 ) ) ;
#2114 = VECTOR ( 'NONE', #7899, 1000.000000000000000 ) ;
#2115 = CARTESIAN_POINT ( 'NONE',  ( 3.015831842038235067, -85.80452850542926058, 3.989209796945429432 ) ) ;
#2116 = CARTESIAN_POINT ( 'NONE',  ( 6.013306294175077227, -64.54547149457073374, -4.245374608440741326 ) ) ;
#2117 = EDGE_CURVE ( 'NONE', #425, #6564, #6175, .T. ) ;
#2118 = CARTESIAN_POINT ( 'NONE',  ( 1.686450176301584003, -65.70452850542925205, -2.482926158054133303 ) ) ;
#2119 = DIRECTION ( 'NONE',  ( 1.000000000000000000, -0.000000000000000000, -0.000000000000000000 ) ) ;
#2120 = DIRECTION ( 'NONE',  ( 0.000000000000000000, 8.673617379884033007E-17, 1.000000000000000000 ) ) ;
#2121 = CARTESIAN_POINT ( 'NONE',  ( -1.686450176301566017, -76.20452850542925205, 2.482926158054133303 ) ) ;
#2122 = CARTESIAN_POINT ( 'NONE',  ( -0.09506052544085988321, -87.00452850542926342, -6.999999999999997335 ) ) ;
#2123 = CARTESIAN_POINT ( 'NONE',  ( 2.369498399071079398, -91.84547149457074511, -6.969112962950057444 ) ) ;
#2124 = DIRECTION ( 'NONE',  ( 1.000000000000000000, 9.251858538542971581E-17, 1.604941620322696727E-32 ) ) ;
#2125 = EDGE_CURVE ( 'NONE', #540, #2326, #318, .T. ) ;
#2126 = DIRECTION ( 'NONE',  ( -1.000000000000000000, -1.261617073437677752E-16, 0.000000000000000000 ) ) ;
#2127 = CARTESIAN_POINT ( 'NONE',  ( -2.493201789345292241, -65.44547149457075363, -1.934965279058240561 ) ) ;
#2128 = SURFACE_SIDE_STYLE ('',( #7818 ) ) ;
#2129 = ORIENTED_EDGE ( 'NONE', *, *, #7263, .F. ) ;
#2130 = CARTESIAN_POINT ( 'NONE',  ( -1.719659006605372964, -72.15452850542921226, -4.969112962950016588 ) ) ;
#2131 = CARTESIAN_POINT ( 'NONE',  ( 6.013306294175077227, -79.54547149457074795, -4.245374608440741326 ) ) ;
#2132 = FILL_AREA_STYLE_COLOUR ( '', #7005 ) ;
#2133 = ORIENTED_EDGE ( 'NONE', *, *, #5412, .F. ) ;
#2134 = VECTOR ( 'NONE', #1852, 1000.000000000000000 ) ;
#2135 = CARTESIAN_POINT ( 'NONE',  ( 0.09506052544085932809, -70.50452850542926342, 4.999999999999997335 ) ) ;
#2136 = DIRECTION ( 'NONE',  ( -1.000000000000000000, -0.000000000000000000, -0.000000000000000000 ) ) ;
#2137 = ADVANCED_FACE ( 'NONE', ( #2897 ), #5462, .T. ) ;
#2138 = CARTESIAN_POINT ( 'NONE',  ( -2.862020680886580681, -74.29547149457074795, -4.100960146803977580 ) ) ;
#2139 = DIRECTION ( 'NONE',  ( -0.000000000000000000, 0.7071067811865507924, 0.7071067811865441310 ) ) ;
#2140 = CARTESIAN_POINT ( 'NONE',  ( 1.529537955723798026, -96.64547149457071384, 5.030887037049945221 ) ) ;
#2141 = CARTESIAN_POINT ( 'NONE',  ( -4.037591185471424815, -64.20452850542925205, 5.718994135553947977 ) ) ;
#2142 = DIRECTION ( 'NONE',  ( -0.9662349396012451797, -0.2576626505603366590, -0.000000000000000000 ) ) ;
#2143 = CARTESIAN_POINT ( 'NONE',  ( 50.00000000000000000, -19.99999999999999645, -12.50000000000000355 ) ) ;
#2144 = CARTESIAN_POINT ( 'NONE',  ( 2.862020680886514956, -83.70452850542925205, -4.100960146804039752 ) ) ;
#2145 = CARTESIAN_POINT ( 'NONE',  ( 0.09506052544088025580, -67.50452850542926342, 6.999999999999997335 ) ) ;
#2146 = EDGE_CURVE ( 'NONE', #5636, #8122, #1818, .T. ) ;
#2147 = CARTESIAN_POINT ( 'NONE',  ( 1.686450176301636183, -78.79547149457074795, 2.482926158054096000 ) ) ;
#2148 = ORIENTED_EDGE ( 'NONE', *, *, #3348, .F. ) ;
#2149 = CIRCLE ( 'NONE', #386, 1.499999999999994449 ) ;
#2150 = DIRECTION ( 'NONE',  ( 0.000000000000000000, -0.7071067811865485719, -0.7071067811865465735 ) ) ;
#2151 = DIRECTION ( 'NONE',  ( -1.000000000000000000, 0.000000000000000000, 0.000000000000000000 ) ) ;
#2152 = CARTESIAN_POINT ( 'NONE',  ( 4.725907263620340082, -77.40452850542925489, -1.635492904037697981 ) ) ;
#2153 = VERTEX_POINT ( 'NONE', #1968 ) ;
#2154 = CARTESIAN_POINT ( 'NONE',  ( -1.719659006605373408, -69.15452850542924068, -4.969112962950015699 ) ) ;
#2155 = CARTESIAN_POINT ( 'NONE',  ( 2.493201789345311781, -90.94547149457073942, 1.934965279058241006 ) ) ;
#2156 = CARTESIAN_POINT ( 'NONE',  ( 2.882544866740875289, -61.39547149457074937, -0.8366430509619593447 ) ) ;
#2157 =( GEOMETRIC_REPRESENTATION_CONTEXT ( 3 ) GLOBAL_UNCERTAINTY_ASSIGNED_CONTEXT ( ( #302 ) ) GLOBAL_UNIT_ASSIGNED_CONTEXT ( ( #4684, #4862, #6834 ) ) REPRESENTATION_CONTEXT ( 'NONE', 'WORKASPACE' ) );
#2158 = CARTESIAN_POINT ( 'NONE',  ( 2.179377348189627472, -60.64547149457074227, 7.030887037049939003 ) ) ;
#2159 = CARTESIAN_POINT ( 'NONE',  ( -1.840261337453253487, -63.30452850542926058, -2.371175808195547852 ) ) ;
#2160 = EDGE_LOOP ( 'NONE', ( #467, #6260, #1887, #3569 ) ) ;
#2161 = LINE ( 'NONE', #5394, #8070 ) ;
#2162 = PLANE ( 'NONE',  #7408 ) ;
#2163 = CARTESIAN_POINT ( 'NONE',  ( 2.493201789345271369, -74.55452850542926058, -1.934965279058294518 ) ) ;
#2164 = CARTESIAN_POINT ( 'NONE',  ( 5.895805022753407343, -89.55452850542926058, -4.407101234057908989 ) ) ;
#2165 = CARTESIAN_POINT ( 'NONE',  ( 4.037591185471564259, -90.79547149457074795, 5.718994135553860936 ) ) ;
#2166 = LINE ( 'NONE', #5482, #6827 ) ;
#2167 = CARTESIAN_POINT ( 'NONE',  ( 40.00000000000000000, -9.999999999999991118, 9.499999999999998224 ) ) ;
#2168 = CARTESIAN_POINT ( 'NONE',  ( -2.610703060766927042, -66.04547149457074795, 1.773238653441125745 ) ) ;
#2169 = UNCERTAINTY_MEASURE_WITH_UNIT (LENGTH_MEASURE( 1.000000000000000082E-05 ), #902, 'distance_accuracy_value', 'NONE');
#2170 = EDGE_LOOP ( 'NONE', ( #5540, #6001, #8319, #4192 ) ) ;
#2171 = EDGE_CURVE ( 'NONE', #5374, #2526, #3101, .T. ) ;
#2172 = CARTESIAN_POINT ( 'NONE',  ( 2.862020680886513180, -68.70452850542925205, -4.100960146804039752 ) ) ;
#2173 = CARTESIAN_POINT ( 'NONE',  ( 6.686770931921477867, -76.39547149457074227, -2.072711028461788896 ) ) ;
#2174 = FILL_AREA_STYLE ('',( #2050 ) ) ;
#2175 = EDGE_LOOP ( 'NONE', ( #5491, #5086, #7142, #7162 ) ) ;
#2176 = CARTESIAN_POINT ( 'NONE',  ( 5.257311121191341918, -68.25452850542926342, -0.09995255151729465215 ) ) ;
#2177 = LINE ( 'NONE', #5411, #864 ) ;
#2178 = EDGE_CURVE ( 'NONE', #5519, #3650, #1842, .T. ) ;
#2179 = CARTESIAN_POINT ( 'NONE',  ( -4.194503406049384431, -68.44547149457073942, -3.171033256558012159 ) ) ;
#2180 = DIRECTION ( 'NONE',  ( 0.000000000000000000, -3.469446951953615175E-16, -1.000000000000000000 ) ) ;
#2181 = CARTESIAN_POINT ( 'NONE',  ( -1.069819614139476460, -63.34547149457073800, 2.969112962950044121 ) ) ;
#2182 = CARTESIAN_POINT ( 'NONE',  ( 4.037591185471440802, -59.70452850542925916, -5.718994135553947977 ) ) ;
#2183 = ORIENTED_EDGE ( 'NONE', *, *, #226, .T. ) ;
#2184 = CYLINDRICAL_SURFACE ( 'NONE', #5842, 6.000000000000000000 ) ;
#2185 = CARTESIAN_POINT ( 'NONE',  ( -3.015831842038214194, -81.30452850542926058, -3.989209796945429432 ) ) ;
#2186 = CARTESIAN_POINT ( 'NONE',  ( -2.369498399071207739, -63.15452850542925489, -6.969112962950009482 ) ) ;
#2187 = CARTESIAN_POINT ( 'NONE',  ( 1.840261337453219959, -73.69547149457073942, -2.371175808195584267 ) ) ;
#2188 = VERTEX_POINT ( 'NONE', #6970 ) ;
#2189 = CARTESIAN_POINT ( 'NONE',  ( -1.500000000000001110, -27.00000000000000000, 5.000000000000000000 ) ) ;
#2190 = LINE ( 'NONE', #74, #6378 ) ;
#2191 = CARTESIAN_POINT ( 'NONE',  ( -4.725907263620321430, -75.90452850542925489, 1.635492904037698647 ) ) ;
#2192 = ORIENTED_EDGE ( 'NONE', *, *, #70, .F. ) ;
#2193 = CARTESIAN_POINT ( 'NONE',  ( 4.312004677471075631, -70.95452850542925205, 3.009306630940844052 ) ) ;
#2194 = CARTESIAN_POINT ( 'NONE',  ( -3.154386672714787565, -92.74547149457073658, -0.09995255151720625064 ) ) ;
#2195 = CARTESIAN_POINT ( 'NONE',  ( 0.09506052544077400746, -58.99547149457073658, -2.999999999999997780 ) ) ;
#2196 = CARTESIAN_POINT ( 'NONE',  ( -2.862020680886494972, -73.20452850542925205, 4.100960146804039752 ) ) ;
#2197 = CARTESIAN_POINT ( 'NONE',  ( 0.09506052544088325340, -91.50452850542926342, 6.999999999999997335 ) ) ;
#2198 = CARTESIAN_POINT ( 'NONE',  ( -3.154386672714791118, -66.75452850542926342, 0.09995255151727280851 ) ) ;
#2199 = VECTOR ( 'NONE', #5732, 1000.000000000000000 ) ;
#2200 = EDGE_LOOP ( 'NONE', ( #1298, #7014, #1856, #8055 ) ) ;
#2201 = LINE ( 'NONE', #3538, #932 ) ;
#2202 = DIRECTION ( 'NONE',  ( -0.000000000000000000, -0.000000000000000000, -1.000000000000000000 ) ) ;
#2203 = CARTESIAN_POINT ( 'NONE',  ( 2.610703060766983885, -79.95452850542925205, 1.773238653441072232 ) ) ;
#2204 = CARTESIAN_POINT ( 'NONE',  ( 2.179377348189483143, -89.85452850542924352, -7.030887037049986077 ) ) ;
#2205 = CARTESIAN_POINT ( 'NONE',  ( -2.369498399071055861, -87.34547149457073090, 6.969112962950058332 ) ) ;
#2206 = EDGE_CURVE ( 'NONE', #4617, #2910, #7590, .T. ) ;
#2207 = LINE ( 'NONE', #4719, #1728 ) ;
#2208 = LINE ( 'NONE', #2839, #2619 ) ;
#2209 = CARTESIAN_POINT ( 'NONE',  ( -1.840261337453201529, -69.19547149457073942, 2.371175808195584267 ) ) ;
#2210 = PRESENTATION_LAYER_ASSIGNMENT (  '', '', ( #5824 ) ) ;
#2211 = DIRECTION ( 'NONE',  ( -0.000000000000000000, -0.000000000000000000, -1.000000000000000000 ) ) ;
#2212 = AXIS2_PLACEMENT_3D ( 'NONE', #321, #3995, #6684 ) ;
#2213 = ORIENTED_EDGE ( 'NONE', *, *, #3070, .T. ) ;
#2214 = CARTESIAN_POINT ( 'NONE',  ( -4.784657899331191011, -66.60452850542924352, -1.454677039711773867 ) ) ;
#2215 = CARTESIAN_POINT ( 'NONE',  ( -6.628020296210667794, -80.59547149457075932, -2.253526892787471869 ) ) ;
#2216 = LINE ( 'NONE', #7351, #7943 ) ;
#2217 = CARTESIAN_POINT ( 'NONE',  ( -4.784657899331158148, -74.89547149457074227, 1.454677039711874675 ) ) ;
#2218 = VECTOR ( 'NONE', #1071, 1000.000000000000000 ) ;
#2219 = CARTESIAN_POINT ( 'NONE',  ( 5.257311121191341918, -65.25452850542926342, -0.09995255151729465215 ) ) ;
#2220 = AXIS2_PLACEMENT_3D ( 'NONE', #6296, #1196, #7091 ) ;
#2221 = LINE ( 'NONE', #7269, #6382 ) ;
#2222 = AXIS2_PLACEMENT_3D ( 'NONE', #3044, #591, #550 ) ;
#2223 = AXIS2_PLACEMENT_3D ( 'NONE', #6216, #1675, #441 ) ;
#2224 = CARTESIAN_POINT ( 'NONE',  ( -4.725907263620355181, -65.59547149457073090, -1.635492904037597617 ) ) ;
#2225 = DIRECTION ( 'NONE',  ( -0.000000000000000000, -0.7071067811865507924, -0.7071067811865441310 ) ) ;
#2226 = CARTESIAN_POINT ( 'NONE',  ( 4.784657899331179465, -94.39547149457074227, -1.454677039711874009 ) ) ;
#2227 = CARTESIAN_POINT ( 'NONE',  ( -6.686770931921507177, -60.60452850542926484, -2.072711028461647675 ) ) ;
#2228 = ORIENTED_EDGE ( 'NONE', *, *, #1545, .T. ) ;
#2229 = CARTESIAN_POINT ( 'NONE',  ( 1.500000000000002442, -27.00000000000000000, 2.500000000000000888 ) ) ;
#2230 = EDGE_CURVE ( 'NONE', #5781, #5070, #3898, .T. ) ;
#2231 = EDGE_LOOP ( 'NONE', ( #8196, #4744, #7445, #5754, #7625 ) ) ;
#2232 = CARTESIAN_POINT ( 'NONE',  ( 54.99999999999999289, -19.99999999999999645, -7.500000000000006217 ) ) ;
#2233 = CARTESIAN_POINT ( 'NONE',  ( -4.312004677471056979, -84.45452850542922363, -3.009306630940844052 ) ) ;
#2234 = CARTESIAN_POINT ( 'NONE',  ( -4.784657899331190123, -81.60452850542925773, -1.454677039711773867 ) ) ;
#2235 = EDGE_LOOP ( 'NONE', ( #334, #7577, #2698, #5736 ) ) ;
#2236 = CARTESIAN_POINT ( 'NONE',  ( 2.862020680886513624, -71.70452850542925205, -4.100960146804039752 ) ) ;
#2237 = CARTESIAN_POINT ( 'NONE',  ( -2.610703060766926153, -78.04547149457074795, 1.773238653441125745 ) ) ;
#2238 = CARTESIAN_POINT ( 'NONE',  ( 3.015831842038151134, -94.69547149457075363, -3.989209796945492048 ) ) ;
#2239 = CARTESIAN_POINT ( 'NONE',  ( 2.862020680886514512, -77.70452850542926626, -4.100960146804039752 ) ) ;
#2240 = CARTESIAN_POINT ( 'NONE',  ( -2.179377348189459607, -91.35452850542925773, 7.030887037049988741 ) ) ;
#2241 = CARTESIAN_POINT ( 'NONE',  ( -2.823794231030038571, -95.59547149457074511, -1.017458915287723364 ) ) ;
#2242 = EDGE_CURVE ( 'NONE', #7184, #604, #2591, .T. ) ;
#2243 = ORIENTED_EDGE ( 'NONE', *, *, #83, .T. ) ;
#2244 = DIRECTION ( 'NONE',  ( 1.000000000000000000, 0.000000000000000000, -0.000000000000000000 ) ) ;
#2245 = ORIENTED_EDGE ( 'NONE', *, *, #2667, .T. ) ;
#2246 = FACE_OUTER_BOUND ( 'NONE', #816, .T. ) ;
#2247 = CARTESIAN_POINT ( 'NONE',  ( -2.610703060766964345, -81.45452850542925205, -1.773238653441072232 ) ) ;
#2248 = CARTESIAN_POINT ( 'NONE',  ( -6.686770931921504513, -84.60452850542927195, -2.072711028461647675 ) ) ;
#2249 = CARTESIAN_POINT ( 'NONE',  ( -6.013306294175058575, -81.04547149457074795, 4.245374608440741326 ) ) ;
#2250 = CARTESIAN_POINT ( 'NONE',  ( -80.00000000000000000, -47.00000000000000711, 12.49999999999999289 ) ) ;
#2251 = CARTESIAN_POINT ( 'NONE',  ( -4.312004677470990366, -96.04547149457074795, 3.009306630940933314 ) ) ;
#2252 = CARTESIAN_POINT ( 'NONE',  ( 2.493201789345272701, -86.55452850542926058, -1.934965279058294518 ) ) ;
#2253 = UNCERTAINTY_MEASURE_WITH_UNIT (LENGTH_MEASURE( 1.000000000000000082E-05 ), #7434, 'distance_accuracy_value', 'NONE');
#2254 = DIRECTION ( 'NONE',  ( -9.251858538542971581E-17, 1.000000000000000000, 0.000000000000000000 ) ) ;
#2255 = ORIENTED_EDGE ( 'NONE', *, *, #937, .F. ) ;
#2256 = DIRECTION ( 'NONE',  ( 1.000000000000000000, 0.000000000000000000, 0.000000000000000000 ) ) ;
#2257 = CARTESIAN_POINT ( 'NONE',  ( 0.09506052544085932809, -70.50452850542926342, 4.999999999999997335 ) ) ;
#2258 = CARTESIAN_POINT ( 'NONE',  ( -6.686770931921458327, -80.89547149457074227, 2.072711028461789784 ) ) ;
#2259 = VERTEX_POINT ( 'NONE', #3268 ) ;
#2260 = CARTESIAN_POINT ( 'NONE',  ( 3.015831842038148469, -73.69547149457073942, -3.989209796945492048 ) ) ;
#2261 = CARTESIAN_POINT ( 'NONE',  ( -3.015831842038130262, -66.19547149457075363, 3.989209796945492048 ) ) ;
#2262 = CARTESIAN_POINT ( 'NONE',  ( -3.015831842038216859, -63.30452850542925347, -3.989209796945429432 ) ) ;
#2263 = DIRECTION ( 'NONE',  ( 0.000000000000000000, 0.000000000000000000, -1.000000000000000000 ) ) ;
#2264 = CARTESIAN_POINT ( 'NONE',  ( -4.784657899331158148, -74.89547149457074227, 1.454677039711874675 ) ) ;
#2265 = CIRCLE ( 'NONE', #8315, 1.500000000000001998 ) ;
#2266 = CARTESIAN_POINT ( 'NONE',  ( 47.49999999999999289, -198.2344135219424857, -12.50000000000005151 ) ) ;
#2267 = CARTESIAN_POINT ( 'NONE',  ( -4.191402346623180897, -60.30452850542926058, -5.607243785695311900 ) ) ;
#2268 = ORIENTED_EDGE ( 'NONE', *, *, #5676, .T. ) ;
#2269 = CARTESIAN_POINT ( 'NONE',  ( 6.123233995736760366E-16, -26.99999999999998934, -7.000000000000000000 ) ) ;
#2270 = ORIENTED_EDGE ( 'NONE', *, *, #7335, .T. ) ;
#2271 = CARTESIAN_POINT ( 'NONE',  ( 75.00000000000000000, -20.00000000000000000, 7.500000000000000000 ) ) ;
#2272 = CARTESIAN_POINT ( 'NONE',  ( -1.719659006605371188, -84.15452850542925489, -4.969112962950016588 ) ) ;
#2273 = CARTESIAN_POINT ( 'NONE',  ( 1.719659006605391172, -76.65452850542922647, 4.969112962950016588 ) ) ;
#2274 = ORIENTED_EDGE ( 'NONE', *, *, #6302, .T. ) ;
#2275 = CARTESIAN_POINT ( 'NONE',  ( -4.194503406049319594, -67.05452850542926058, 3.171033256558101865 ) ) ;
#2276 = CARTESIAN_POINT ( 'NONE',  ( -2.882544866740857969, -77.89547149457074227, 0.8366430509619596778 ) ) ;
#2277 = CARTESIAN_POINT ( 'NONE',  ( -4.784657899331155484, -95.89547149457074227, 1.454677039711874675 ) ) ;
#2278 = CARTESIAN_POINT ( 'NONE',  ( -5.257311121191324155, -72.75452850542924921, 0.09995255151729526277 ) ) ;
#2279 = CARTESIAN_POINT ( 'NONE',  ( -4.037591185471421262, -91.20452850542925205, 5.718994135553947977 ) ) ;
#2280 = CARTESIAN_POINT ( 'NONE',  ( 1.069819614139497332, -97.84547149457073090, -2.969112962950042789 ) ) ;
#2281 = EDGE_CURVE ( 'NONE', #2962, #7308, #3774, .T. ) ;
#2282 = VECTOR ( 'NONE', #6481, 1000.000000000000000 ) ;
#2283 = ORIENTED_EDGE ( 'NONE', *, *, #7691, .T. ) ;
#2284 = DIRECTION ( 'NONE',  ( 1.000000000000000000, 0.000000000000000000, 0.000000000000000000 ) ) ;
#2285 = LINE ( 'NONE', #295, #2295 ) ;
#2286 = CARTESIAN_POINT ( 'NONE',  ( 0.8796985632578976366, -65.85452850542924352, -3.030887037049972310 ) ) ;
#2287 = EDGE_CURVE ( 'NONE', #5238, #8124, #2354, .T. ) ;
#2288 = CARTESIAN_POINT ( 'NONE',  ( 4.312004677471013459, -88.54547149457074795, -3.009306630940932425 ) ) ;
#2289 =( GEOMETRIC_REPRESENTATION_CONTEXT ( 3 ) GLOBAL_UNCERTAINTY_ASSIGNED_CONTEXT ( ( #5541 ) ) GLOBAL_UNIT_ASSIGNED_CONTEXT ( ( #1740, #4299, #3082 ) ) REPRESENTATION_CONTEXT ( 'NONE', 'WORKASPACE' ) );
#2290 = CARTESIAN_POINT ( 'NONE',  ( -2.179377348189610153, -83.14547149457072805, -7.030887037049939003 ) ) ;
#2291 = DIRECTION ( 'NONE',  ( 0.000000000000000000, 0.000000000000000000, 1.000000000000000000 ) ) ;
#2292 = APPLICATION_CONTEXT ( 'automotive_design' ) ;
#2293 = CARTESIAN_POINT ( 'NONE',  ( 4.194503406049403083, -93.94547149457075363, 3.171033256558012159 ) ) ;
#2294 = CARTESIAN_POINT ( 'NONE',  ( 2.823794231030042123, -89.40452850542926910, -1.017458915287783316 ) ) ;
#2295 = VECTOR ( 'NONE', #1563, 1000.000000000000000 ) ;
#2296 = DIRECTION ( 'NONE',  ( 0.000000000000000000, 0.000000000000000000, -1.000000000000000000 ) ) ;
#2297 = ORIENTED_EDGE ( 'NONE', *, *, #5110, .T. ) ;
#2298 = CARTESIAN_POINT ( 'NONE',  ( -80.00000000000000000, -2.168404344971008868E-15, 12.50000000000000000 ) ) ;
#2299 = CARTESIAN_POINT ( 'NONE',  ( -0.09506052544081705635, -93.00452850542926342, -2.999999999999997780 ) ) ;
#2300 = CARTESIAN_POINT ( 'NONE',  ( 6.013306294175077227, -67.54547149457074795, -4.245374608440741326 ) ) ;
#2301 = SHAPE_REPRESENTATION_RELATIONSHIP ( 'NONE' , 'NONE' ,  #1066, #3582 ) ;
#2302 = EDGE_LOOP ( 'NONE', ( #1741, #7262 ) ) ;
#2303 = CARTESIAN_POINT ( 'NONE',  ( 1.529537955723795584, -78.64547149457074227, 5.030887037049945221 ) ) ;
#2304 = CARTESIAN_POINT ( 'NONE',  ( 5.257311121191341918, -70.24547149457075079, 0.09995255151718437925 ) ) ;
#2305 = CARTESIAN_POINT ( 'NONE',  ( 4.194503406049335581, -68.55452850542926058, -3.171033256558100089 ) ) ;
#2306 = CARTESIAN_POINT ( 'NONE',  ( 6.000000000000007105, -50.00000000000000000, -2.499999999999999112 ) ) ;
#2307 = CARTESIAN_POINT ( 'NONE',  ( -1.529537955723777598, -74.14547149457074227, -5.030887037049945221 ) ) ;
#2308 = EDGE_CURVE ( 'NONE', #996, #2188, #643, .T. ) ;
#2309 = CARTESIAN_POINT ( 'NONE',  ( -0.09506052544083770650, -96.00452850542926342, -4.999999999999997335 ) ) ;
#2310 = ORIENTED_EDGE ( 'NONE', *, *, #602, .F. ) ;
#2311 = DIRECTION ( 'NONE',  ( -1.000000000000000000, 0.000000000000000000, -0.000000000000000000 ) ) ;
#2312 = EDGE_LOOP ( 'NONE', ( #2228, #1882 ) ) ;
#2313 = CARTESIAN_POINT ( 'NONE',  ( -80.00000000000000000, -25.00000000000000000, -20.00000000000000000 ) ) ;
#2314 = CARTESIAN_POINT ( 'NONE',  ( 4.725907263620341858, -89.40452850542926910, -1.635492904037697981 ) ) ;
#2315 = CARTESIAN_POINT ( 'NONE',  ( -0.09506052544083998246, -78.00452850542926342, -4.999999999999997335 ) ) ;
#2316 = CARTESIAN_POINT ( 'NONE',  ( 4.784657899331207886, -59.10452850542925773, 1.454677039711774533 ) ) ;
#2317 = CARTESIAN_POINT ( 'NONE',  ( 0.8796985632579624736, -81.64547149457074227, 3.030887037049952326 ) ) ;
#2318 = CARTESIAN_POINT ( 'NONE',  ( -1.840261337453202639, -60.19547149457074653, 2.371175808195584267 ) ) ;
#2319 = CARTESIAN_POINT ( 'NONE',  ( 4.725907263620340082, -68.40452850542925489, -1.635492904037697981 ) ) ;
#2320 = CARTESIAN_POINT ( 'NONE',  ( 2.369498399071227279, -91.65452850542924068, 6.969112962950009482 ) ) ;
#2321 = CARTESIAN_POINT ( 'NONE',  ( -2.610703060766967010, -60.45452850542925916, -1.773238653441072232 ) ) ;
#2322 = APPLICATION_PROTOCOL_DEFINITION ( 'draft international standard', 'automotive_design', 1998, #5020 ) ;
#2323 = ORIENTED_EDGE ( 'NONE', *, *, #2035, .F. ) ;
#2324 = CARTESIAN_POINT ( 'NONE',  ( 6.000000000000006217, -47.00000000000000000, -2.499999999999999112 ) ) ;
#2325 = PRODUCT_DEFINITION_SHAPE ( 'NONE', 'NONE',  #8342 ) ;
#2326 = VERTEX_POINT ( 'NONE', #5199 ) ;
#2327 = DIRECTION ( 'NONE',  ( 0.000000000000000000, 0.000000000000000000, 1.000000000000000000 ) ) ;
#2328 = CARTESIAN_POINT ( 'NONE',  ( 0.09506052544083769262, -67.50452850542926342, 2.999999999999997780 ) ) ;
#2329 = CARTESIAN_POINT ( 'NONE',  ( -6.686770931921459216, -77.89547149457074227, 2.072711028461789784 ) ) ;
#2330 = LINE ( 'NONE', #463, #5485 ) ;
#2331 = CARTESIAN_POINT ( 'NONE',  ( -5.257311121191322378, -92.74547149457073658, -0.09995255151718372699 ) ) ;
#2332 = CARTESIAN_POINT ( 'NONE',  ( -1.840261337453249935, -90.30452850542926058, -2.371175808195547852 ) ) ;
#2333 = SURFACE_STYLE_FILL_AREA ( #2843 ) ;
#2334 = EDGE_LOOP ( 'NONE', ( #181, #6990 ) ) ;
#2335 = CARTESIAN_POINT ( 'NONE',  ( 0.7729879516809982087, -29.89870481880373987, 2.500000000000000888 ) ) ;
#2336 = CARTESIAN_POINT ( 'NONE',  ( -3.154386672714787565, -93.75452850542926342, 0.09995255151727280851 ) ) ;
#2337 = CARTESIAN_POINT ( 'NONE',  ( 7.360235569667877620, -70.24547149457075079, 0.09995255151716216091 ) ) ;
#2338 = CARTESIAN_POINT ( 'NONE',  ( 1.023909817990208637, -97.00000000000002842, -5.931815031828092444 ) ) ;
#2339 = CARTESIAN_POINT ( 'NONE',  ( -0.09506052544073578803, -72.49547149457075079, 4.999999999999997335 ) ) ;
#2340 = CARTESIAN_POINT ( 'NONE',  ( 3.015831842038148469, -73.69547149457073942, -3.989209796945492048 ) ) ;
#2341 = CARTESIAN_POINT ( 'NONE',  ( -2.862020680886496304, -61.20452850542925205, 4.100960146804039752 ) ) ;
#2342 = DIRECTION ( 'NONE',  ( 0.000000000000000000, -1.000000000000000000, -2.168404344971009854E-16 ) ) ;
#2343 = AXIS2_PLACEMENT_3D ( 'NONE', #3856, #7147, #7610 ) ;
#2344 = EDGE_CURVE ( 'NONE', #4647, #6779, #3826, .T. ) ;
#2345 = ADVANCED_FACE ( 'NONE', ( #5658, #7099 ), #6345, .T. ) ;
#2346 = CARTESIAN_POINT ( 'NONE',  ( 0.09506052544075337118, -61.99547149457074369, -4.999999999999997335 ) ) ;
#2347 =( LENGTH_UNIT ( ) NAMED_UNIT ( * ) SI_UNIT ( .MILLI., .METRE. ) );
#2348 = VECTOR ( 'NONE', #5444, 1000.000000000000000 ) ;
#2349 = CARTESIAN_POINT ( 'NONE',  ( -1.719659006605370744, -93.15452850542925489, -4.969112962950016588 ) ) ;
#2350 = ORIENTED_EDGE ( 'NONE', *, *, #1548, .T. ) ;
#2351 = MECHANICAL_DESIGN_GEOMETRIC_PRESENTATION_REPRESENTATION (  '', ( #5975 ), #725 ) ;
#2352 = UNCERTAINTY_MEASURE_WITH_UNIT (LENGTH_MEASURE( 1.000000000000000082E-05 ), #1034, 'distance_accuracy_value', 'NONE');
#2353 = FACE_BOUND ( 'NONE', #7797, .T. ) ;
#2354 = CIRCLE ( 'NONE', #319, 1.500000000000001332 ) ;
#2355 = ORIENTED_EDGE ( 'NONE', *, *, #3890, .T. ) ;
#2356 = DIRECTION ( 'NONE',  ( 1.000000000000000000, 0.000000000000000000, 0.000000000000000000 ) ) ;
#2357 = CARTESIAN_POINT ( 'NONE',  ( 0.09506052544086084077, -82.50452850542926342, 4.999999999999997335 ) ) ;
#2358 = CARTESIAN_POINT ( 'NONE',  ( -4.194503406049382654, -92.44547149457073942, -3.171033256558012159 ) ) ;
#2359 = CARTESIAN_POINT ( 'NONE',  ( 2.862020680886512736, -65.70452850542925205, -4.100960146804039752 ) ) ;
#2360 = CARTESIAN_POINT ( 'NONE',  ( 2.823794231030060331, -82.09547149457075932, 1.017458915287723809 ) ) ;
#2361 = CARTESIAN_POINT ( 'NONE',  ( -0.09506052544073390065, -87.49547149457075079, 4.999999999999997335 ) ) ;
#2362 = CARTESIAN_POINT ( 'NONE',  ( -1.719659006605373630, -66.15452850542926910, -4.969112962950016588 ) ) ;
#2363 = CARTESIAN_POINT ( 'NONE',  ( 6.686770931921524941, -83.10452850542927195, 2.072711028461649008 ) ) ;
#2364 = CARTESIAN_POINT ( 'NONE',  ( 2.882544866740879730, -94.39547149457074227, -0.8366430509619593447 ) ) ;
#2365 = ORIENTED_EDGE ( 'NONE', *, *, #5011, .F. ) ;
#2366 = DIRECTION ( 'NONE',  ( 0.000000000000000000, -1.000000000000000000, 8.673617379884034239E-17 ) ) ;
#2367 = ORIENTED_EDGE ( 'NONE', *, *, #3717, .T. ) ;
#2368 = CARTESIAN_POINT ( 'NONE',  ( 1.529537955723691889, -86.85452850542924352, -5.030887037049978971 ) ) ;
#2369 = CARTESIAN_POINT ( 'NONE',  ( -0.8796985632578802061, -70.35452850542922931, 3.030887037049973198 ) ) ;
#2370 = EDGE_CURVE ( 'NONE', #3916, #4621, #562, .T. ) ;
#2371 = CARTESIAN_POINT ( 'NONE',  ( -2.369498399071057637, -75.34547149457073090, 6.969112962950058332 ) ) ;
#2372 = CARTESIAN_POINT ( 'NONE',  ( 4.194503406049339134, -92.55452850542924637, -3.171033256558100089 ) ) ;
#2373 = LINE ( 'NONE', #4175, #2348 ) ;
#2374 = CARTESIAN_POINT ( 'NONE',  ( -1.840261337453250157, -87.30452850542926058, -2.371175808195547852 ) ) ;
#2375 = FACE_OUTER_BOUND ( 'NONE', #3074, .T. ) ;
#2376 = ORIENTED_EDGE ( 'NONE', *, *, #7403, .F. ) ;
#2377 = CARTESIAN_POINT ( 'NONE',  ( 5.257311121191341918, -59.25452850542924210, -0.09995255151729465215 ) ) ;
#2378 = CARTESIAN_POINT ( 'NONE',  ( 0.09506052544073390065, -73.99547149457075079, -6.999999999999997335 ) ) ;
#2379 = EDGE_CURVE ( 'NONE', #3352, #2522, #2509, .T. ) ;
#2380 =( LENGTH_UNIT ( ) NAMED_UNIT ( * ) SI_UNIT ( .MILLI., .METRE. ) );
#2381 = FACE_OUTER_BOUND ( 'NONE', #1036, .T. ) ;
#2382 = CARTESIAN_POINT ( 'NONE',  ( 4.725907263620372945, -76.09547149457074511, 1.635492904037598283 ) ) ;
#2383 = CARTESIAN_POINT ( 'NONE',  ( -2.862020680886581125, -71.29547149457074795, -4.100960146803977580 ) ) ;
#2384 = CARTESIAN_POINT ( 'NONE',  ( -4.725907263620324095, -57.90452850542925489, 1.635492904037698647 ) ) ;
#2385 = DIRECTION ( 'NONE',  ( 0.000000000000000000, 0.000000000000000000, 1.000000000000000000 ) ) ;
#2386 = CARTESIAN_POINT ( 'NONE',  ( -4.725907263620322318, -66.90452850542925489, 1.635492904037698647 ) ) ;
#2387 = CARTESIAN_POINT ( 'NONE',  ( 5.257311121191341918, -61.24547149457074369, 0.09995255151718437925 ) ) ;
#2388 = VERTEX_POINT ( 'NONE', #1885 ) ;
#2389 = LINE ( 'NONE', #4991, #7200 ) ;
#2390 = VERTEX_POINT ( 'NONE', #4432 ) ;
#2391 = DIRECTION ( 'NONE',  ( -1.261617073437677752E-16, 1.000000000000000000, 0.000000000000000000 ) ) ;
#2392 = CARTESIAN_POINT ( 'NONE',  ( 3.015831842038235067, -85.80452850542926058, 3.989209796945429432 ) ) ;
#2393 = EDGE_CURVE ( 'NONE', #5386, #1649, #4518, .T. ) ;
#2394 = CARTESIAN_POINT ( 'NONE',  ( 4.784657899331179465, -91.39547149457075648, -1.454677039711874009 ) ) ;
#2395 = CARTESIAN_POINT ( 'NONE',  ( 4.784657899331208775, -65.10452850542924352, 1.454677039711774533 ) ) ;
#2396 = CARTESIAN_POINT ( 'NONE',  ( 2.882544866740878398, -85.39547149457074227, -0.8366430509619593447 ) ) ;
#2397 = CARTESIAN_POINT ( 'NONE',  ( -6.686770931921504513, -81.60452850542927195, -2.072711028461647675 ) ) ;
#2398 = CARTESIAN_POINT ( 'NONE',  ( 1.529537955723796028, -84.64547149457074227, 5.030887037049945221 ) ) ;
#2399 = EDGE_CURVE ( 'NONE', #3118, #4154, #5737, .T. ) ;
#2400 = CARTESIAN_POINT ( 'NONE',  ( -4.784657899331191011, -66.60452850542924352, -1.454677039711773867 ) ) ;
#2401 = CARTESIAN_POINT ( 'NONE',  ( 4.191402346623198660, -82.80452850542926058, 5.607243785695311900 ) ) ;
#2402 = CARTESIAN_POINT ( 'NONE',  ( 2.493201789345269148, -59.55452850542924637, -1.934965279058294518 ) ) ;
#2403 = ORIENTED_EDGE ( 'NONE', *, *, #7183, .F. ) ;
#2404 = CARTESIAN_POINT ( 'NONE',  ( 80.00000000000000000, -25.00000000000000000, 20.00000000000000000 ) ) ;
#2405 = EDGE_LOOP ( 'NONE', ( #4179, #3289, #4917, #1860 ) ) ;
#2406 = CARTESIAN_POINT ( 'NONE',  ( -4.725907263620319654, -90.90452850542926910, 1.635492904037698647 ) ) ;
#2407 = CARTESIAN_POINT ( 'NONE',  ( -2.610703060766965677, -72.45452850542925205, -1.773238653441072232 ) ) ;
#2408 = CARTESIAN_POINT ( 'NONE',  ( -0.09506052544086367184, -57.00452850542925631, -6.999999999999997335 ) ) ;
#2409 = CARTESIAN_POINT ( 'NONE',  ( 0.09506052544073312349, -67.99547149457075079, -6.999999999999997335 ) ) ;
#2410 = CARTESIAN_POINT ( 'NONE',  ( 3.015831842038149802, -82.69547149457073942, -3.989209796945492048 ) ) ;
#2411 = CARTESIAN_POINT ( 'NONE',  ( -2.610703060766963901, -84.45452850542925205, -1.773238653441072232 ) ) ;
#2412 = CARTESIAN_POINT ( 'NONE',  ( 54.99999999999999289, -20.00000000000000000, 7.500000000000000000 ) ) ;
#2413 = ORIENTED_EDGE ( 'NONE', *, *, #6523, .F. ) ;
#2414 =( LENGTH_UNIT ( ) NAMED_UNIT ( * ) SI_UNIT ( .MILLI., .METRE. ) );
#2415 = CARTESIAN_POINT ( 'NONE',  ( 0.09506052544085819012, -61.50452850542925631, 4.999999999999997335 ) ) ;
#2416 = AXIS2_PLACEMENT_3D ( 'NONE', #294, #7894, #2911 ) ;
#2417 = CARTESIAN_POINT ( 'NONE',  ( 6.686770931921476979, -70.39547149457072805, -2.072711028461788896 ) ) ;
#2418 = SURFACE_STYLE_FILL_AREA ( #6249 ) ;
#2419 = CARTESIAN_POINT ( 'NONE',  ( -80.00000000000000000, -50.00000000000000711, 12.49999999999999289 ) ) ;
#2420 = CARTESIAN_POINT ( 'NONE',  ( 3.015831842038147137, -64.69547149457075363, -3.989209796945492048 ) ) ;
#2421 = CARTESIAN_POINT ( 'NONE',  ( 1.719659006605283924, -64.84547149457071669, -4.969112962950050338 ) ) ;
#2422 = CARTESIAN_POINT ( 'NONE',  ( 2.493201789345273589, -92.55452850542926058, -1.934965279058294518 ) ) ;
#2423 = PLANE ( 'NONE',  #5437 ) ;
#2424 = PRODUCT_DEFINITION_FORMATION_WITH_SPECIFIED_SOURCE ( 'ANY', '', #3664, .NOT_KNOWN. ) ;
#2425 = CARTESIAN_POINT ( 'NONE',  ( -0.09506052544084110656, -69.00452850542926342, -4.999999999999997335 ) ) ;
#2426 = VECTOR ( 'NONE', #7312, 1000.000000000000000 ) ;
#2427 = CARTESIAN_POINT ( 'NONE',  ( 6.686770931921480532, -97.39547149457074227, -2.072711028461788896 ) ) ;
#2428 = ORIENTED_EDGE ( 'NONE', *, *, #3717, .F. ) ;
#2429 = EDGE_CURVE ( 'NONE', #1573, #7540, #58, .T. ) ;
#2430 = CARTESIAN_POINT ( 'NONE',  ( 40.00000000000000000, -9.999999999999992895, 4.499999999999999112 ) ) ;
#2431 = VERTEX_POINT ( 'NONE', #603 ) ;
#2432 = FACE_OUTER_BOUND ( 'NONE', #3201, .T. ) ;
#2433 = CARTESIAN_POINT ( 'NONE',  ( -1.529537955723670795, -73.35452850542922931, 5.030887037049979860 ) ) ;
#2434 = CARTESIAN_POINT ( 'NONE',  ( -4.194503406049382654, -89.44547149457073942, -3.171033256558012159 ) ) ;
#2435 = CARTESIAN_POINT ( 'NONE',  ( -2.862020680886495860, -64.20452850542926626, 4.100960146804039752 ) ) ;
#2436 = CARTESIAN_POINT ( 'NONE',  ( 2.493201789345308672, -66.94547149457073942, 1.934965279058241006 ) ) ;
#2437 = CARTESIAN_POINT ( 'NONE',  ( 6.628020296210642037, -83.40452850542925489, -2.253526892787612645 ) ) ;
#2438 = CARTESIAN_POINT ( 'NONE',  ( 4.312004677471013459, -91.54547149457074795, -3.009306630940933314 ) ) ;
#2439 = CARTESIAN_POINT ( 'NONE',  ( -4.194503406049319594, -70.05452850542923215, 3.171033256558100533 ) ) ;
#2440 = CARTESIAN_POINT ( 'NONE',  ( 6.013306294175169597, -79.95452850542925205, 4.245374608440616093 ) ) ;
#2441 = CARTESIAN_POINT ( 'NONE',  ( -2.882544866740855749, -89.89547149457074227, 0.8366430509619596778 ) ) ;
#2442 = ORIENTED_EDGE ( 'NONE', *, *, #4590, .T. ) ;
#2443 = FACE_OUTER_BOUND ( 'NONE', #1282, .T. ) ;
#2444 = DIRECTION ( 'NONE',  ( -0.000000000000000000, -0.000000000000000000, -1.000000000000000000 ) ) ;
#2445 = ORIENTED_EDGE ( 'NONE', *, *, #7652, .T. ) ;
#2446 = CARTESIAN_POINT ( 'NONE',  ( -5.257311121191322378, -87.75452850542923500, 0.09995255151729529053 ) ) ;
#2447 = CARTESIAN_POINT ( 'NONE',  ( -2.882544866740878398, -69.60452850542924352, -0.8366430509618996147 ) ) ;
#2448 = EDGE_CURVE ( 'NONE', #524, #5519, #8279, .T. ) ;
#2449 = CARTESIAN_POINT ( 'NONE',  ( 2.862020680886516732, -95.70452850542926626, -4.100960146804039752 ) ) ;
#2450 = CARTESIAN_POINT ( 'NONE',  ( -4.191402346623058328, -69.19547149457073942, 5.607243785695398941 ) ) ;
#2451 = CARTESIAN_POINT ( 'NONE',  ( 4.194503406049403083, -81.94547149457073942, 3.171033256558012159 ) ) ;
#2452 = CARTESIAN_POINT ( 'NONE',  ( 2.882544866740897049, -80.10452850542927195, 0.8366430509618999478 ) ) ;
#2453 = FACE_OUTER_BOUND ( 'NONE', #3610, .T. ) ;
#2454 = VERTEX_POINT ( 'NONE', #1923 ) ;
#2455 = CARTESIAN_POINT ( 'NONE',  ( 43.45299461620743386, 65.00000000000000000, -7.500000000000000000 ) ) ;
#2456 = CARTESIAN_POINT ( 'NONE',  ( 2.493201789345274033, -95.55452850542926058, -1.934965279058294518 ) ) ;
#2457 = CARTESIAN_POINT ( 'NONE',  ( 2.179377348189629249, -75.64547149457072805, 7.030887037049939003 ) ) ;
#2458 = EDGE_CURVE ( 'NONE', #7988, #8240, #7187, .T. ) ;
#2459 = DIRECTION ( 'NONE',  ( 0.000000000000000000, 0.000000000000000000, 1.000000000000000000 ) ) ;
#2460 = CARTESIAN_POINT ( 'NONE',  ( 4.366652375515289286, -96.99999999999995737, 2.564342289837593380 ) ) ;
#2461 = CARTESIAN_POINT ( 'NONE',  ( 4.784657899331176800, -67.39547149457074227, -1.454677039711874009 ) ) ;
#2462 = CARTESIAN_POINT ( 'NONE',  ( -3.015831842038130706, -63.19547149457074653, 3.989209796945492048 ) ) ;
#2463 = CARTESIAN_POINT ( 'NONE',  ( -1.686450176301563353, -94.20452850542928047, 2.482926158054133303 ) ) ;
#2464 = DIRECTION ( 'NONE',  ( 0.000000000000000000, 0.000000000000000000, -1.000000000000000000 ) ) ;
#2465 = CARTESIAN_POINT ( 'NONE',  ( 5.257311121191341918, -68.25452850542926342, -0.09995255151729465215 ) ) ;
#2466 = CARTESIAN_POINT ( 'NONE',  ( -7.360235569667856304, -95.74547149457073658, -0.09995255151716124498 ) ) ;
#2467 = ORIENTED_EDGE ( 'NONE', *, *, #7477, .T. ) ;
#2468 = ADVANCED_FACE ( 'NONE', ( #6044 ), #2768, .T. ) ;
#2469 = DIRECTION ( 'NONE',  ( 1.000000000000000000, 0.000000000000000000, 0.000000000000000000 ) ) ;
#2470 =( LENGTH_UNIT ( ) NAMED_UNIT ( * ) SI_UNIT ( .MILLI., .METRE. ) );
#2471 = ORIENTED_EDGE ( 'NONE', *, *, #6088, .T. ) ;
#2472 = AXIS2_PLACEMENT_3D ( 'NONE', #938, #5448, #2254 ) ;
#2473 = LINE ( 'NONE', #4277, #4084 ) ;
#2474 = CARTESIAN_POINT ( 'NONE',  ( 3.015831842038234178, -79.80452850542926058, 3.989209796945429432 ) ) ;
#2475 = CIRCLE ( 'NONE', #7188, 3.000000000000002665 ) ;
#2476 = CARTESIAN_POINT ( 'NONE',  ( -5.257311121191323267, -86.74547149457072237, -0.09995255151718371311 ) ) ;
#2477 = CARTESIAN_POINT ( 'NONE',  ( -1.719659006605374518, -60.15452850542926200, -4.969112962950015699 ) ) ;
#2478 = CARTESIAN_POINT ( 'NONE',  ( 1.686450176301634851, -66.79547149457073374, 2.482926158054096000 ) ) ;
#2479 = CARTESIAN_POINT ( 'NONE',  ( -5.895805022753386027, -76.05452850542926058, 4.407101234057909878 ) ) ;
#2480 = CARTESIAN_POINT ( 'NONE',  ( -1.529537955723776044, -86.14547149457074227, -5.030887037049945221 ) ) ;
#2481 = CARTESIAN_POINT ( 'NONE',  ( -1.529537955723671683, -64.35452850542924352, 5.030887037049979860 ) ) ;
#2482 = CARTESIAN_POINT ( 'NONE',  ( -7.360235569667858968, -78.75452850542926342, 0.09995255151731782806 ) ) ;
#2483 = CIRCLE ( 'NONE', #1953, 0.9999999999999948930 ) ;
#2484 = CARTESIAN_POINT ( 'NONE',  ( 3.154386672714810658, -88.24547149457073658, 0.09995255151720662534 ) ) ;
#2485 = EDGE_CURVE ( 'NONE', #7988, #2655, #5329, .T. ) ;
#2486 = ORIENTED_EDGE ( 'NONE', *, *, #8250, .T. ) ;
#2487 = DIRECTION ( 'NONE',  ( 0.000000000000000000, 0.000000000000000000, -1.000000000000000000 ) ) ;
#2488 = CARTESIAN_POINT ( 'NONE',  ( 54.99999999999999289, -20.00000000000000000, 7.500000000000000000 ) ) ;
#2489 = ORIENTED_EDGE ( 'NONE', *, *, #4223, .T. ) ;
#2490 = CARTESIAN_POINT ( 'NONE',  ( 4.194503406049340022, -95.55452850542924637, -3.171033256558100977 ) ) ;
#2491 = CARTESIAN_POINT ( 'NONE',  ( 3.154386672714806217, -59.25452850542926342, -0.09995255151727241993 ) ) ;
#2492 = CARTESIAN_POINT ( 'NONE',  ( -5.257311121191321490, -93.75452850542926342, 0.09995255151729526277 ) ) ;
#2493 = CARTESIAN_POINT ( 'NONE',  ( -5.895805022753479285, -71.44547149457072521, -4.407101234057782868 ) ) ;
#2494 = CARTESIAN_POINT ( 'NONE',  ( 5.257311121191342806, -85.24547149457075079, 0.09995255151718437925 ) ) ;
#2495 = CARTESIAN_POINT ( 'NONE',  ( -1.840261337453251933, -75.30452850542926058, -2.371175808195547852 ) ) ;
#2496 = EDGE_LOOP ( 'NONE', ( #6830, #3490, #8007, #2721 ) ) ;
#2497 = DIRECTION ( 'NONE',  ( -0.000000000000000000, 1.000000000000000000, 2.775557561562891351E-16 ) ) ;
#2498 = CARTESIAN_POINT ( 'NONE',  ( 3.154386672714809770, -86.25452850542924921, -0.09995255151727241993 ) ) ;
#2499 = CARTESIAN_POINT ( 'NONE',  ( 6.013306294175077227, -64.54547149457073374, -4.245374608440741326 ) ) ;
#2500 = CARTESIAN_POINT ( 'NONE',  ( 4.827973024309449634, -96.99999999999998579, 2.218963830005241444 ) ) ;
#2501 = CARTESIAN_POINT ( 'NONE',  ( 0.09506052544075374588, -64.99547149457075079, -4.999999999999997335 ) ) ;
#2502 = CARTESIAN_POINT ( 'NONE',  ( -2.862020680886582014, -62.29547149457074084, -4.100960146803977580 ) ) ;
#2503 = CARTESIAN_POINT ( 'NONE',  ( -4.312004677471061420, -57.45452850542925916, -3.009306630940844052 ) ) ;
#2504 = CARTESIAN_POINT ( 'NONE',  ( 80.00000000000000000, -9.999999999999994671, 0.000000000000000000 ) ) ;
#2505 = CARTESIAN_POINT ( 'NONE',  ( -4.194503406049319594, -67.05452850542926058, 3.171033256558100533 ) ) ;
#2506 = CARTESIAN_POINT ( 'NONE',  ( 5.895805022753498825, -96.94547149457073942, 4.407101234057782868 ) ) ;
#2507 = FILL_AREA_STYLE ('',( #7013 ) ) ;
#2508 = EDGE_LOOP ( 'NONE', ( #7523, #6131, #8016, #5417 ) ) ;
#2509 = LINE ( 'NONE', #7736, #6911 ) ;
#2510 = ORIENTED_EDGE ( 'NONE', *, *, #4629, .T. ) ;
#2511 = DIRECTION ( 'NONE',  ( 0.000000000000000000, 0.000000000000000000, 1.000000000000000000 ) ) ;
#2512 = CARTESIAN_POINT ( 'NONE',  ( -4.784657899331190123, -75.60452850542925773, -1.454677039711773867 ) ) ;
#2513 = CARTESIAN_POINT ( 'NONE',  ( 5.257311121191341918, -85.24547149457075079, 0.09995255151718437925 ) ) ;
#2514 = CARTESIAN_POINT ( 'NONE',  ( 4.277672441867257369, -96.99999999999992895, 1.818343915288929136 ) ) ;
#2515 = CARTESIAN_POINT ( 'NONE',  ( -3.154386672714790674, -74.74547149457073658, -0.09995255151720625064 ) ) ;
#2516 = CARTESIAN_POINT ( 'NONE',  ( 5.895805022753406455, -77.55452850542926058, -4.407101234057908989 ) ) ;
#2517 = CARTESIAN_POINT ( 'NONE',  ( -4.725907263620351628, -89.59547149457074511, -1.635492904037597617 ) ) ;
#2518 = PLANE ( 'NONE',  #5073 ) ;
#2519 = CARTESIAN_POINT ( 'NONE',  ( 0.09506052544088212930, -82.50452850542926342, 6.999999999999997335 ) ) ;
#2520 = CARTESIAN_POINT ( 'NONE',  ( -1.069819614139472463, -90.34547149457073090, 2.969112962950044121 ) ) ;
#2521 = ADVANCED_FACE ( 'NONE', ( #5959 ), #7824, .T. ) ;
#2522 = VERTEX_POINT ( 'NONE', #6550 ) ;
#2523 = CARTESIAN_POINT ( 'NONE',  ( 54.99999999999999289, -20.00000000000000000, 7.499999999999993783 ) ) ;
#2524 = LINE ( 'NONE', #5088, #4898 ) ;
#2525 = PRODUCT ( 'jaw', 'jaw', '', ( #5784 ) ) ;
#2526 = VERTEX_POINT ( 'NONE', #3477 ) ;
#2527 = CARTESIAN_POINT ( 'NONE',  ( 4.725907263620341858, -86.40452850542926910, -1.635492904037697981 ) ) ;
#2528 = CARTESIAN_POINT ( 'NONE',  ( 3.154386672714807105, -62.25452850542926342, -0.09995255151727241993 ) ) ;
#2529 = VECTOR ( 'NONE', #1317, 1000.000000000000000 ) ;
#2530 = CARTESIAN_POINT ( 'NONE',  ( 1.719659006605392504, -94.65452850542921226, 4.969112962950016588 ) ) ;
#2531 = CARTESIAN_POINT ( 'NONE',  ( 4.191402346623077868, -70.69547149457073942, -5.607243785695398941 ) ) ;
#2532 = EDGE_CURVE ( 'NONE', #4976, #7927, #2483, .T. ) ;
#2533 = CARTESIAN_POINT ( 'NONE',  ( -3.015831842038127153, -90.19547149457073942, 3.989209796945492048 ) ) ;
#2534 = CARTESIAN_POINT ( 'NONE',  ( -2.823794231030020807, -78.90452850542925489, 1.017458915287783316 ) ) ;
#2535 = DIRECTION ( 'NONE',  ( -0.8660254037844380415, -0.5000000000000011102, 0.000000000000000000 ) ) ;
#2536 =( NAMED_UNIT ( * ) SI_UNIT ( $, .STERADIAN. ) SOLID_ANGLE_UNIT ( ) );
#2537 = CARTESIAN_POINT ( 'NONE',  ( 1.840261337453272583, -88.80452850542926058, 2.371175808195547852 ) ) ;
#2538 = CARTESIAN_POINT ( 'NONE',  ( 0.09506052544073236021, -61.99547149457073658, -6.999999999999997335 ) ) ;
#2539 = DIRECTION ( 'NONE',  ( 0.000000000000000000, 0.000000000000000000, -1.000000000000000000 ) ) ;
#2540 = CARTESIAN_POINT ( 'NONE',  ( -4.312004677470993919, -69.04547149457071953, 3.009306630940933314 ) ) ;
#2541 = CARTESIAN_POINT ( 'NONE',  ( -4.725907263620356069, -59.59547149457074511, -1.635492904037597617 ) ) ;
#2542 = CARTESIAN_POINT ( 'NONE',  ( 1.840261337453272805, -91.80452850542926058, 2.371175808195547852 ) ) ;
#2543 = DIRECTION ( 'NONE',  ( 0.000000000000000000, -2.775557561562891351E-16, 1.000000000000000000 ) ) ;
#2544 = VECTOR ( 'NONE', #1442, 1000.000000000000000 ) ;
#2545 = CIRCLE ( 'NONE', #4825, 0.9999999999999948930 ) ;
#2546 = CARTESIAN_POINT ( 'NONE',  ( 3.015831842038232402, -64.80452850542926058, 3.989209796945429432 ) ) ;
#2547 = CARTESIAN_POINT ( 'NONE',  ( 6.686770931921479644, -94.39547149457074227, -2.072711028461788896 ) ) ;
#2548 = ORIENTED_EDGE ( 'NONE', *, *, #2242, .F. ) ;
#2549 = AXIS2_PLACEMENT_3D ( 'NONE', #1388, #2072, #3959 ) ;
#2550 = VECTOR ( 'NONE', #3673, 1000.000000000000000 ) ;
#2551 = CARTESIAN_POINT ( 'NONE',  ( 54.99999999999999289, 80.00000000000000000, 7.500000000000000000 ) ) ;
#2552 = SHAPE_DEFINITION_REPRESENTATION ( #8309, #6502 ) ;
#2553 = VECTOR ( 'NONE', #4545, 1000.000000000000000 ) ;
#2554 = ADVANCED_FACE ( 'NONE', ( #4064, #3354 ), #188, .T. ) ;
#2555 = EDGE_LOOP ( 'NONE', ( #3396, #7430 ) ) ;
#2556 = DIRECTION ( 'NONE',  ( -0.000000000000000000, -0.000000000000000000, -1.000000000000000000 ) ) ;
#2557 = CARTESIAN_POINT ( 'NONE',  ( 1.719659006605391172, -76.65452850542922647, 4.969112962950016588 ) ) ;
#2558 = CARTESIAN_POINT ( 'NONE',  ( -0.09506052544073466393, -81.49547149457075079, 4.999999999999997335 ) ) ;
#2559 = CARTESIAN_POINT ( 'NONE',  ( 2.919221509273758119, -96.99999999999992895, -2.847688208160571666 ) ) ;
#2560 = CARTESIAN_POINT ( 'NONE',  ( 2.610703060766944361, -70.54547149457074795, -1.773238653441125523 ) ) ;
#2561 = CARTESIAN_POINT ( 'NONE',  ( -2.369498399071206407, -81.15452850542924068, -6.969112962950009482 ) ) ;
#2562 = CARTESIAN_POINT ( 'NONE',  ( 4.784657899331178577, -82.39547149457074227, -1.454677039711874009 ) ) ;
#2563 = CARTESIAN_POINT ( 'NONE',  ( -4.312004677471060532, -60.45452850542923784, -3.009306630940844052 ) ) ;
#2564 = DIRECTION ( 'NONE',  ( 0.000000000000000000, 2.775557561562891351E-16, -1.000000000000000000 ) ) ;
#2565 = CARTESIAN_POINT ( 'NONE',  ( -2.179377348189461383, -79.35452850542927195, 7.030887037049988741 ) ) ;
#2566 = CARTESIAN_POINT ( 'NONE',  ( -3.154386672714789341, -83.74547149457075079, -0.09995255151720625064 ) ) ;
#2567 = EDGE_LOOP ( 'NONE', ( #1431, #3511, #2951, #899 ) ) ;
#2568 = CARTESIAN_POINT ( 'NONE',  ( -3.999999999999988898, -87.00000000000001421, 4.898587196589412829E-16 ) ) ;
#2569 = CARTESIAN_POINT ( 'NONE',  ( -1.529537955723779374, -59.14547149457073516, -5.030887037049945221 ) ) ;
#2570 = ORIENTED_EDGE ( 'NONE', *, *, #6134, .T. ) ;
#2571 = CARTESIAN_POINT ( 'NONE',  ( -4.312004677471057867, -78.45452850542925205, -3.009306630940843608 ) ) ;
#2572 = CARTESIAN_POINT ( 'NONE',  ( -1.686450176301568016, -58.20452850542925916, 2.482926158054133303 ) ) ;
#2573 = CARTESIAN_POINT ( 'NONE',  ( -6.686770931921508954, -57.60452850542926484, -2.072711028461647675 ) ) ;
#2574 = CARTESIAN_POINT ( 'NONE',  ( -6.628020296210667794, -68.59547149457073090, -2.253526892787471869 ) ) ;
#2575 = CARTESIAN_POINT ( 'NONE',  ( -4.312004677470991254, -90.04547149457073374, 3.009306630940933314 ) ) ;
#2576 = CARTESIAN_POINT ( 'NONE',  ( 1.686450176301585335, -74.70452850542925205, -2.482926158054133303 ) ) ;
#2577 = DIRECTION ( 'NONE',  ( 1.000000000000000000, -0.000000000000000000, -0.000000000000000000 ) ) ;
#2578 = CARTESIAN_POINT ( 'NONE',  ( 50.00000000000000000, -9.999999999999991118, 9.499999999999998224 ) ) ;
#2579 = CARTESIAN_POINT ( 'NONE',  ( -2.493201789345250496, -88.05452850542926058, 1.934965279058294518 ) ) ;
#2580 = CARTESIAN_POINT ( 'NONE',  ( -6.013306294175062128, -60.04547149457073374, 4.245374608440741326 ) ) ;
#2581 = LINE ( 'NONE', #2630, #3756 ) ;
#2582 = CARTESIAN_POINT ( 'NONE',  ( -3.015831842038130706, -63.19547149457074653, 3.989209796945492048 ) ) ;
#2583 = CARTESIAN_POINT ( 'NONE',  ( -4.194503406049384431, -59.44547149457074653, -3.171033256558012159 ) ) ;
#2584 = LINE ( 'NONE', #5904, #2529 ) ;
#2585 = CARTESIAN_POINT ( 'NONE',  ( 63.45299461620744808, 100.0000000000000000, 7.500000000000000000 ) ) ;
#2586 = CARTESIAN_POINT ( 'NONE',  ( 4.784657899331207886, -59.10452850542925773, 1.454677039711774533 ) ) ;
#2587 = CARTESIAN_POINT ( 'NONE',  ( 2.369498399071078953, -88.84547149457073090, -6.969112962950057444 ) ) ;
#2588 =( NAMED_UNIT ( * ) SI_UNIT ( $, .STERADIAN. ) SOLID_ANGLE_UNIT ( ) );
#2589 = ORIENTED_EDGE ( 'NONE', *, *, #5149, .T. ) ;
#2590 = CARTESIAN_POINT ( 'NONE',  ( 1.529537955723689224, -71.85452850542925773, -5.030887037049978971 ) ) ;
#2591 = LINE ( 'NONE', #687, #3960 ) ;
#2592 = EDGE_CURVE ( 'NONE', #8018, #943, #7870, .T. ) ;
#2593 = VECTOR ( 'NONE', #1962, 1000.000000000000000 ) ;
#2594 = ADVANCED_FACE ( 'NONE', ( #4778 ), #2726, .T. ) ;
#2595 = ITEM_DEFINED_TRANSFORMATION ( 'NONE', 'NONE', #5907,  #2840 ) ;
#2596 = DIRECTION ( 'NONE',  ( 0.000000000000000000, 0.000000000000000000, 1.000000000000000000 ) ) ;
#2597 = CARTESIAN_POINT ( 'NONE',  ( 4.725907263620372945, -76.09547149457074511, 1.635492904037598283 ) ) ;
#2598 = CARTESIAN_POINT ( 'NONE',  ( 2.480136385090595308, -96.99999999999992895, -3.206978988282922050 ) ) ;
#2599 = CARTESIAN_POINT ( 'NONE',  ( 2.610703060766944361, -67.54547149457074795, -1.773238653441125523 ) ) ;
#2600 = CARTESIAN_POINT ( 'NONE',  ( -7.360235569667858968, -72.75452850542926342, 0.09995255151731782806 ) ) ;
#2601 = DIRECTION ( 'NONE',  ( -9.251858538542971581E-17, 1.000000000000000000, 0.000000000000000000 ) ) ;
#2602 = CARTESIAN_POINT ( 'NONE',  ( -4.194503406049384431, -80.44547149457073942, -3.171033256558012159 ) ) ;
#2603 = APPLICATION_CONTEXT ( 'automotive_design' ) ;
#2604 = CARTESIAN_POINT ( 'NONE',  ( -65.00000000000000000, 0.000000000000000000, 0.000000000000000000 ) ) ;
#2605 = CARTESIAN_POINT ( 'NONE',  ( -4.784657899331188347, -93.60452850542925773, -1.454677039711773867 ) ) ;
#2606 = CARTESIAN_POINT ( 'NONE',  ( 2.179377348189480479, -65.85452850542924352, -7.030887037049986077 ) ) ;
#2607 = CARTESIAN_POINT ( 'NONE',  ( 1.686450176301635961, -75.79547149457074795, 2.482926158054096000 ) ) ;
#2608 = VECTOR ( 'NONE', #3187, 1000.000000000000000 ) ;
#2609 = ORIENTED_EDGE ( 'NONE', *, *, #843, .T. ) ;
#2610 = DIRECTION ( 'NONE',  ( -0.09506052544079829358, 0.9954714945707483498, 0.000000000000000000 ) ) ;
#2611 = CARTESIAN_POINT ( 'NONE',  ( 50.00000000000000000, -1.734723475976807094E-15, 12.50000000000000000 ) ) ;
#2612 = CARTESIAN_POINT ( 'NONE',  ( -4.725907263620319654, -87.90452850542926910, 1.635492904037698647 ) ) ;
#2613 = ORIENTED_EDGE ( 'NONE', *, *, #5114, .F. ) ;
#2614 = CARTESIAN_POINT ( 'NONE',  ( 4.194503406049339134, -80.55452850542926058, -3.171033256558100977 ) ) ;
#2615 = CARTESIAN_POINT ( 'NONE',  ( 1.840261337453222845, -97.69547149457076785, -2.371175808195584267 ) ) ;
#2616 = CARTESIAN_POINT ( 'NONE',  ( 0.000000000000000000, 0.000000000000000000, 0.000000000000000000 ) ) ;
#2617 = VECTOR ( 'NONE', #1750, 1000.000000000000000 ) ;
#2618 = CARTESIAN_POINT ( 'NONE',  ( -2.862020680886492752, -88.20452850542925205, 4.100960146804039752 ) ) ;
#2619 = VECTOR ( 'NONE', #935, 1000.000000000000000 ) ;
#2620 = PRESENTATION_LAYER_ASSIGNMENT (  '', '', ( #5975 ) ) ;
#2621 = CARTESIAN_POINT ( 'NONE',  ( -4.037591185471546495, -62.29547149457074084, -5.718994135553860936 ) ) ;
#2622 = CARTESIAN_POINT ( 'NONE',  ( -4.312004677470992142, -81.04547149457071953, 3.009306630940933314 ) ) ;
#2623 = CARTESIAN_POINT ( 'NONE',  ( 3.154386672714808437, -71.25452850542926342, -0.09995255151727241993 ) ) ;
#2624 = VECTOR ( 'NONE', #6763, 1000.000000000000000 ) ;
#2625 = DIRECTION ( 'NONE',  ( 0.000000000000000000, 0.000000000000000000, 1.000000000000000000 ) ) ;
#2626 = EDGE_CURVE ( 'NONE', #1554, #204, #7868, .T. ) ;
#2627 = CARTESIAN_POINT ( 'NONE',  ( 65.00000000000000000, 0.000000000000000000, 0.000000000000000000 ) ) ;
#2628 = CARTESIAN_POINT ( 'NONE',  ( -1.686450176301564685, -85.20452850542925205, 2.482926158054133303 ) ) ;
#2629 = CARTESIAN_POINT ( 'NONE',  ( 4.037591185471445243, -95.70452850542928047, -5.718994135553947977 ) ) ;
#2630 = CARTESIAN_POINT ( 'NONE',  ( 54.99999999999999289, -30.00000000000000000, -7.500000000000007105 ) ) ;
#2631 = CARTESIAN_POINT ( 'NONE',  ( -0.09506052544083960776, -81.00452850542926342, -4.999999999999997335 ) ) ;
#2632 = CARTESIAN_POINT ( 'NONE',  ( 4.037591185471565147, -96.79547149457073374, 5.718994135553860936 ) ) ;
#2633 = CARTESIAN_POINT ( 'NONE',  ( -5.999999999999995559, -27.99999999999999645, 2.500000000000000888 ) ) ;
#2634 = DIRECTION ( 'NONE',  ( 0.000000000000000000, 1.734723475976806108E-16, 1.000000000000000000 ) ) ;
#2635 = CLOSED_SHELL ( 'NONE', ( #1037, #4519, #4754, #4844, #6356, #7819, #6759, #2594, #7467, #277, #4433 ) ) ;
#2636 = CARTESIAN_POINT ( 'NONE',  ( 5.257311121191341918, -59.25452850542924210, -0.09995255151729465215 ) ) ;
#2637 = EDGE_CURVE ( 'NONE', #1922, #549, #4649, .T. ) ;
#2638 = CARTESIAN_POINT ( 'NONE',  ( 2.369498399071079398, -91.84547149457074511, -6.969112962950057444 ) ) ;
#2639 = PRESENTATION_STYLE_ASSIGNMENT (( #5821 ) ) ;
#2640 = ORIENTED_EDGE ( 'NONE', *, *, #113, .T. ) ;
#2641 = CARTESIAN_POINT ( 'NONE',  ( 4.312004677471074743, -70.95452850542925205, 3.009306630940844496 ) ) ;
#2642 = DIRECTION ( 'NONE',  ( -0.000000000000000000, -0.000000000000000000, 1.000000000000000000 ) ) ;
#2643 = LINE ( 'NONE', #1888, #6776 ) ;
#2644 = CARTESIAN_POINT ( 'NONE',  ( -0.09506052544073541333, -75.49547149457073658, 4.999999999999997335 ) ) ;
#2645 = CARTESIAN_POINT ( 'NONE',  ( 3.534712008015381102, -97.00000000000002842, -2.138372830837821148 ) ) ;
#2646 = CARTESIAN_POINT ( 'NONE',  ( -2.823794231030041235, -65.59547149457073090, -1.017458915287723364 ) ) ;
#2647 = CARTESIAN_POINT ( 'NONE',  ( -4.037591185471423927, -70.20452850542925205, 5.718994135553947977 ) ) ;
#2648 = DIRECTION ( 'NONE',  ( 0.000000000000000000, 1.734723475976806108E-16, 1.000000000000000000 ) ) ;
#2649 = CARTESIAN_POINT ( 'NONE',  ( -1.529537955723777154, -77.14547149457074227, -5.030887037049945221 ) ) ;
#2650 = CARTESIAN_POINT ( 'NONE',  ( 1.719659006605388507, -61.65452850542923358, 4.969112962950016588 ) ) ;
#2651 = CARTESIAN_POINT ( 'NONE',  ( 4.194503406049339134, -86.55452850542926058, -3.171033256558100089 ) ) ;
#2652 = CARTESIAN_POINT ( 'NONE',  ( 4.191402346623196884, -70.80452850542926058, 5.607243785695311900 ) ) ;
#2653 = CARTESIAN_POINT ( 'NONE',  ( 1.840261337453220625, -76.69547149457073942, -2.371175808195584267 ) ) ;
#2654 = EDGE_CURVE ( 'NONE', #5682, #970, #1453, .T. ) ;
#2655 = VERTEX_POINT ( 'NONE', #3401 ) ;
#2656 = CARTESIAN_POINT ( 'NONE',  ( -5.999999999999992895, -50.00000000000000000, -2.499999999999999112 ) ) ;
#2657 = CARTESIAN_POINT ( 'NONE',  ( -4.194503406049314265, -94.05452850542926058, 3.171033256558100533 ) ) ;
#2658 = CARTESIAN_POINT ( 'NONE',  ( 2.862020680886516288, -92.70452850542926626, -4.100960146804039752 ) ) ;
#2659 = EDGE_LOOP ( 'NONE', ( #8266, #1257, #5282, #4966 ) ) ;
#2660 = CARTESIAN_POINT ( 'NONE',  ( -2.862020680886493196, -85.20452850542925205, 4.100960146804039752 ) ) ;
#2661 = CARTESIAN_POINT ( 'NONE',  ( 1.840261337453268808, -61.80452850542926058, 2.371175808195547852 ) ) ;
#2662 = CARTESIAN_POINT ( 'NONE',  ( -4.312004677471056091, -90.45452850542926626, -3.009306630940844052 ) ) ;
#2663 = CARTESIAN_POINT ( 'NONE',  ( -7.360235569667860744, -59.74547149457073658, -0.09995255151716124498 ) ) ;
#2664 = CARTESIAN_POINT ( 'NONE',  ( 2.493201789345270480, -68.55452850542926058, -1.934965279058294518 ) ) ;
#2665 = LINE ( 'NONE', #1438, #3761 ) ;
#2666 = AXIS2_PLACEMENT_3D ( 'NONE', #3430, #2838, #6745 ) ;
#2667 = EDGE_CURVE ( 'NONE', #2388, #4058, #2221, .T. ) ;
#2668 = DIRECTION ( 'NONE',  ( 0.000000000000000000, 0.000000000000000000, 1.000000000000000000 ) ) ;
#2669 = CARTESIAN_POINT ( 'NONE',  ( -1.840261337453249935, -90.30452850542926058, -2.371175808195547852 ) ) ;
#2670 = CARTESIAN_POINT ( 'NONE',  ( 2.369498399071227723, -94.65452850542924068, 6.969112962950009482 ) ) ;
#2671 = CARTESIAN_POINT ( 'NONE',  ( 50.00000000000000000, -9.999999999999994671, 0.000000000000000000 ) ) ;
#2672 = B_SPLINE_CURVE_WITH_KNOTS ( 'NONE', 3,
 ( #3679, #4262, #2338, #553, #1873, #1746, #8152, #6835, #1067, #5610, #6960, #6876, #3089, #6373, #3173, #5649, #472, #4304, #3640, #6250, #6919, #6206, #1787, #2500, #8189, #1154, #8229, #430, #8111, #2460, #3003, #3722 ),
 .UNSPECIFIED., .F., .F.,
 ( 4, 2, 2, 2, 2, 2, 2, 2, 2, 2, 2, 2, 2, 2, 2, 4 ),
 ( 0.000000000000000000, 0.001531221420384391721, 0.002296832130576588124, 0.003062442840768784310, 0.004593664261153176248, 0.005359274971345372868, 0.006124885681537568620, 0.007656107101921958390, 0.009187328522306347292, 0.009952939232498542177, 0.01071854994269073533, 0.01148416065288293195, 0.01186696600797902852, 0.01205836868552707768, 0.01215407002430110225, 0.01224977136307512857 ),
 .UNSPECIFIED. ) ;
#2673 = CARTESIAN_POINT ( 'NONE',  ( -4.312004677471057867, -78.45452850542925205, -3.009306630940844052 ) ) ;
#2674 = CARTESIAN_POINT ( 'NONE',  ( 2.179377348189631469, -93.64547149457074227, 7.030887037049939003 ) ) ;
#2675 = CARTESIAN_POINT ( 'NONE',  ( 80.00000000000000000, 0.000000000000000000, 0.000000000000000000 ) ) ;
#2676 = CARTESIAN_POINT ( 'NONE',  ( 43.45299461620743386, 65.00000000000000000, -7.500000000000000000 ) ) ;
#2677 = CARTESIAN_POINT ( 'NONE',  ( 0.09506052544077515931, -67.99547149457075079, -2.999999999999997780 ) ) ;
#2678 = CARTESIAN_POINT ( 'NONE',  ( 2.862020680886511848, -59.70452850542925205, -4.100960146804039752 ) ) ;
#2679 = CARTESIAN_POINT ( 'NONE',  ( 2.179377348189631469, -93.64547149457074227, 7.030887037049939003 ) ) ;
#2680 = EDGE_LOOP ( 'NONE', ( #281, #7421 ) ) ;
#2681 = CARTESIAN_POINT ( 'NONE',  ( -0.09506052544083998246, -78.00452850542926342, -4.999999999999997335 ) ) ;
#2682 = CARTESIAN_POINT ( 'NONE',  ( 0.000000000000000000, -9.999999999999994671, -34.24264068711928388 ) ) ;
#2683 = CIRCLE ( 'NONE', #5901, 4.000000000000000000 ) ;
#2684 = AXIS2_PLACEMENT_3D ( 'NONE', #6539, #631, #3215 ) ;
#2685 = CARTESIAN_POINT ( 'NONE',  ( 54.99999999999999289, -9.999999999999994671, 0.000000000000000000 ) ) ;
#2686 = CARTESIAN_POINT ( 'NONE',  ( -2.369498399071058081, -69.34547149457073090, 6.969112962950058332 ) ) ;
#2687 = CARTESIAN_POINT ( 'NONE',  ( 3.015831842038149357, -79.69547149457075363, -3.989209796945492048 ) ) ;
#2688 = LINE ( 'NONE', #5874, #6857 ) ;
#2689 = CARTESIAN_POINT ( 'NONE',  ( -2.823794231030042567, -59.59547149457074511, -1.017458915287723364 ) ) ;
#2690 = VECTOR ( 'NONE', #4504, 1000.000000000000000 ) ;
#2691 = CARTESIAN_POINT ( 'NONE',  ( -0.09506052544086217304, -69.00452850542926342, -6.999999999999997335 ) ) ;
#2692 = CARTESIAN_POINT ( 'NONE',  ( -47.50000000000000711, -20.00000000000000355, 12.49999999999999112 ) ) ;
#2693 = CARTESIAN_POINT ( 'NONE',  ( 1.529537955723795584, -75.64547149457069963, 5.030887037049945221 ) ) ;
#2694 = CARTESIAN_POINT ( 'NONE',  ( -4.725907263620320542, -84.90452850542925489, 1.635492904037698647 ) ) ;
#2695 = CARTESIAN_POINT ( 'NONE',  ( -6.628020296210622497, -69.90452850542925489, 2.253526892787613978 ) ) ;
#2696 = VECTOR ( 'NONE', #85, 1000.000000000000000 ) ;
#2697 = CARTESIAN_POINT ( 'NONE',  ( 0.09506052544077629729, -76.99547149457075079, -2.999999999999997780 ) ) ;
#2698 = ORIENTED_EDGE ( 'NONE', *, *, #12, .F. ) ;
#2699 = CARTESIAN_POINT ( 'NONE',  ( 46.49999999999999289, -14.99999999999999467, 2.500000000000000888 ) ) ;
#2700 = CARTESIAN_POINT ( 'NONE',  ( -1.499999999999999556, -9.999999999999994671, -30.00000000000000000 ) ) ;
#2701 = CARTESIAN_POINT ( 'NONE',  ( -0.09506052544083846978, -90.00452850542924921, -4.999999999999997335 ) ) ;
#2702 = ORIENTED_EDGE ( 'NONE', *, *, #4820, .T. ) ;
#2703 = CARTESIAN_POINT ( 'NONE',  ( 4.725907263620340970, -83.40452850542925489, -1.635492904037697981 ) ) ;
#2704 = CARTESIAN_POINT ( 'NONE',  ( -1.840261337453198864, -90.19547149457073942, 2.371175808195584267 ) ) ;
#2705 = VECTOR ( 'NONE', #7719, 1000.000000000000000 ) ;
#2706 = CARTESIAN_POINT ( 'NONE',  ( 1.529537955723692111, -89.85452850542925773, -5.030887037049978971 ) ) ;
#2707 = CARTESIAN_POINT ( 'NONE',  ( 2.369498399071227723, -94.65452850542924068, 6.969112962950009482 ) ) ;
#2708 = CARTESIAN_POINT ( 'NONE',  ( 3.154386672714807105, -65.25452850542926342, -0.09995255151727241993 ) ) ;
#2709 = PRESENTATION_LAYER_ASSIGNMENT (  '', '', ( #3102 ) ) ;
#2710 = ADVANCED_FACE ( 'NONE', ( #5869 ), #6507, .F. ) ;
#2711 = CARTESIAN_POINT ( 'NONE',  ( -54.99999999999999289, -100.0000000000000000, 20.00000000000000000 ) ) ;
#2712 = CARTESIAN_POINT ( 'NONE',  ( -5.999999999999993783, -47.00000000000000000, -2.499999999999999112 ) ) ;
#2713 = CARTESIAN_POINT ( 'NONE',  ( -3.154386672714789341, -81.75452850542926342, 0.09995255151727280851 ) ) ;
#2714 = CARTESIAN_POINT ( 'NONE',  ( 2.369498399071225947, -85.65452850542926910, 6.969112962950009482 ) ) ;
#2715 = CARTESIAN_POINT ( 'NONE',  ( 6.123233995736760366E-16, -27.00000000000000000, 4.500000000000000888 ) ) ;
#2716 = CARTESIAN_POINT ( 'NONE',  ( -0.09506052544071189048, -93.49547149457075079, 6.999999999999997335 ) ) ;
#2717 = CARTESIAN_POINT ( 'NONE',  ( 1.097606853890779561E-14, -87.00000000000001421, 0.000000000000000000 ) ) ;
#2718 = CARTESIAN_POINT ( 'NONE',  ( 47.50000000000002132, -54.00000000000000711, -12.50000000000001954 ) ) ;
#2719 = CARTESIAN_POINT ( 'NONE',  ( 2.610703060766944361, -67.54547149457074795, -1.773238653441125523 ) ) ;
#2720 = CARTESIAN_POINT ( 'NONE',  ( 4.725907263620339194, -59.40452850542926200, -1.635492904037697981 ) ) ;
#2721 = ORIENTED_EDGE ( 'NONE', *, *, #3407, .T. ) ;
#2722 = CARTESIAN_POINT ( 'NONE',  ( 4.784657899331208775, -65.10452850542924352, 1.454677039711774533 ) ) ;
#2723 = CARTESIAN_POINT ( 'NONE',  ( 4.191402346623079644, -85.69547149457073942, -5.607243785695398941 ) ) ;
#2724 = ORIENTED_EDGE ( 'NONE', *, *, #353, .F. ) ;
#2725 = CARTESIAN_POINT ( 'NONE',  ( 4.194503406049337357, -77.55452850542926058, -3.171033256558100089 ) ) ;
#2726 = CYLINDRICAL_SURFACE ( 'NONE', #4756, 3.000000000000000000 ) ;
#2727 = CARTESIAN_POINT ( 'NONE',  ( 54.99999999999999289, -9.999999999999994671, 0.000000000000000000 ) ) ;
#2728 = CARTESIAN_POINT ( 'NONE',  ( 4.312004677471012570, -79.54547149457074795, -3.009306630940933314 ) ) ;
#2729 = EDGE_CURVE ( 'NONE', #7693, #2822, #6003, .T. ) ;
#2730 = CARTESIAN_POINT ( 'NONE',  ( 1.499999999999999556, -9.999999999999994671, -34.24264068711928388 ) ) ;
#2731 = CARTESIAN_POINT ( 'NONE',  ( 1.069819614139492447, -61.84547149457074511, -2.969112962950042789 ) ) ;
#2732 = CARTESIAN_POINT ( 'NONE',  ( -4.037591185471423039, -73.20452850542925205, 5.718994135553947977 ) ) ;
#2733 = DIRECTION ( 'NONE',  ( 0.000000000000000000, 0.000000000000000000, -1.000000000000000000 ) ) ;
#2734 = CARTESIAN_POINT ( 'NONE',  ( 4.194503406049402194, -81.94547149457073942, 3.171033256558012159 ) ) ;
#2735 = CARTESIAN_POINT ( 'NONE',  ( -0.09506052544083846978, -90.00452850542924921, -4.999999999999997335 ) ) ;
#2736 = CARTESIAN_POINT ( 'NONE',  ( -7.360235569667858968, -66.75452850542926342, 0.09995255151731782806 ) ) ;
#2737 = CARTESIAN_POINT ( 'NONE',  ( -2.493201789345290464, -80.44547149457073942, -1.934965279058240561 ) ) ;
#2738 = ORIENTED_EDGE ( 'NONE', *, *, #7893, .F. ) ;
#2739 = DIRECTION ( 'NONE',  ( -0.000000000000000000, -0.000000000000000000, -1.000000000000000000 ) ) ;
#2740 = CARTESIAN_POINT ( 'NONE',  ( 0.09506052544086235345, -94.50452850542926342, 4.999999999999997335 ) ) ;
#2741 = CARTESIAN_POINT ( 'NONE',  ( -3.015831842038213750, -87.30452850542926058, -3.989209796945429432 ) ) ;
#2742 = EDGE_CURVE ( 'NONE', #1012, #2766, #2177, .T. ) ;
#2743 = ORIENTED_EDGE ( 'NONE', *, *, #734, .F. ) ;
#2744 = CARTESIAN_POINT ( 'NONE',  ( 4.194503406049338246, -77.55452850542926058, -3.171033256558100977 ) ) ;
#2745 = CARTESIAN_POINT ( 'NONE',  ( -2.823794231030038571, -89.59547149457074511, -1.017458915287723364 ) ) ;
#2746 = CARTESIAN_POINT ( 'NONE',  ( -5.257311121191322378, -87.75452850542922079, 0.09995255151729526277 ) ) ;
#2747 = CARTESIAN_POINT ( 'NONE',  ( 6.686770931921525829, -95.10452850542925773, 2.072711028461649008 ) ) ;
#2748 = VECTOR ( 'NONE', #1802, 1000.000000000000000 ) ;
#2749 = CARTESIAN_POINT ( 'NONE',  ( 2.823794231030039459, -68.40452850542925489, -1.017458915287783316 ) ) ;
#2750 = CARTESIAN_POINT ( 'NONE',  ( 1.223768561234547464E-14, -97.00000000000000000, 0.000000000000000000 ) ) ;
#2751 = FACE_BOUND ( 'NONE', #7838, .T. ) ;
#2752 = CARTESIAN_POINT ( 'NONE',  ( 1.069819614139557729, -82.65452850542926910, 2.969112962950023249 ) ) ;
#2753 = VECTOR ( 'NONE', #2296, 1000.000000000000000 ) ;
#2754 = CARTESIAN_POINT ( 'NONE',  ( 4.037591185471444355, -86.70452850542925205, -5.718994135553947977 ) ) ;
#2755 = VECTOR ( 'NONE', #2556, 1000.000000000000000 ) ;
#2756 = CARTESIAN_POINT ( 'NONE',  ( 6.123233995736760366E-16, -27.00000000000000000, -5.000000000000000000 ) ) ;
#2757 = CARTESIAN_POINT ( 'NONE',  ( 0.09506052544073574639, -88.99547149457075079, -6.999999999999997335 ) ) ;
#2758 = PLANE ( 'NONE',  #8053 ) ;
#2759 = CARTESIAN_POINT ( 'NONE',  ( 50.00000000000000000, -20.00000000000000000, 4.499999999999997335 ) ) ;
#2760 = ADVANCED_FACE ( 'NONE', ( #1537 ), #906, .T. ) ;
#2761 = CARTESIAN_POINT ( 'NONE',  ( -1.840261337453201973, -66.19547149457073942, 2.371175808195584267 ) ) ;
#2762 = AXIS2_PLACEMENT_3D ( 'NONE', #7398, #4187, #3558 ) ;
#2763 = EDGE_LOOP ( 'NONE', ( #6738, #2922, #3529, #440 ) ) ;
#2764 = CARTESIAN_POINT ( 'NONE',  ( 1.529537955723689224, -71.85452850542925773, -5.030887037049978971 ) ) ;
#2765 = CARTESIAN_POINT ( 'NONE',  ( 5.895805022753496161, -81.94547149457073942, 4.407101234057782868 ) ) ;
#2766 = VERTEX_POINT ( 'NONE', #6800 ) ;
#2767 = CARTESIAN_POINT ( 'NONE',  ( 2.862020680886514068, -74.70452850542926626, -4.100960146804039752 ) ) ;
#2768 = PLANE ( 'NONE',  #589 ) ;
#2769 = CONTEXT_DEPENDENT_SHAPE_REPRESENTATION ( #3572, #8113 ) ;
#2770 = CARTESIAN_POINT ( 'NONE',  ( 1.719659006605285478, -73.84547149457074511, -4.969112962950050338 ) ) ;
#2771 = PLANE ( 'NONE',  #8210 ) ;
#2772 = CARTESIAN_POINT ( 'NONE',  ( 1.840261337453218848, -64.69547149457073942, -2.371175808195584267 ) ) ;
#2773 = CARTESIAN_POINT ( 'NONE',  ( -6.013306294175152722, -66.45452850542925205, -4.245374608440613429 ) ) ;
#2774 = CARTESIAN_POINT ( 'NONE',  ( 44.22701204831900412, -12.10129518119625658, 4.500000000000000888 ) ) ;
#2775 = SURFACE_STYLE_USAGE ( .BOTH. , #6641 ) ;
#2776 = CARTESIAN_POINT ( 'NONE',  ( -4.312004677471056979, -84.45452850542922363, -3.009306630940844052 ) ) ;
#2777 = CARTESIAN_POINT ( 'NONE',  ( 6.628020296210639373, -71.40452850542924068, -2.253526892787612645 ) ) ;
#2778 = CARTESIAN_POINT ( 'NONE',  ( -3.154386672714789341, -80.74547149457075079, -0.09995255151720625064 ) ) ;
#2779 = VERTEX_POINT ( 'NONE', #4911 ) ;
#2780 = CARTESIAN_POINT ( 'NONE',  ( 50.00000000000000000, -7.999999999999996447, 12.49999999999999822 ) ) ;
#2781 = CARTESIAN_POINT ( 'NONE',  ( 2.862020680886516288, -92.70452850542926626, -4.100960146804039752 ) ) ;
#2782 = CARTESIAN_POINT ( 'NONE',  ( 5.257311121191341918, -83.25452850542926342, -0.09995255151729465215 ) ) ;
#2783 = EDGE_LOOP ( 'NONE', ( #227, #3912, #3895, #4312 ) ) ;
#2784 = CARTESIAN_POINT ( 'NONE',  ( 1.719659006605390061, -70.65452850542926910, 4.969112962950015699 ) ) ;
#2785 = CARTESIAN_POINT ( 'NONE',  ( 1.840261337453221513, -88.69547149457073942, -2.371175808195584267 ) ) ;
#2786 = CARTESIAN_POINT ( 'NONE',  ( -0.09506052544083884448, -87.00452850542924921, -4.999999999999997335 ) ) ;
#2787 = CARTESIAN_POINT ( 'NONE',  ( -2.179377348189459163, -94.35452850542925773, 7.030887037049988741 ) ) ;
#2788 = CARTESIAN_POINT ( 'NONE',  ( 2.882544866740894829, -65.10452850542924352, 0.8366430509618999478 ) ) ;
#2789 = EDGE_CURVE ( 'NONE', #3705, #9, #3018, .T. ) ;
#2790 = ORIENTED_EDGE ( 'NONE', *, *, #7003, .F. ) ;
#2791 = DIRECTION ( 'NONE',  ( -0.000000000000000000, 0.000000000000000000, -1.000000000000000000 ) ) ;
#2792 = DIRECTION ( 'NONE',  ( -0.000000000000000000, -0.000000000000000000, -1.000000000000000000 ) ) ;
#2793 = CARTESIAN_POINT ( 'NONE',  ( -2.823794231030020807, -78.90452850542925489, 1.017458915287783316 ) ) ;
#2794 = CARTESIAN_POINT ( 'NONE',  ( -0.09506052544085913381, -93.00452850542926342, -6.999999999999997335 ) ) ;
#2795 = EDGE_CURVE ( 'NONE', #4167, #731, #1534, .T. ) ;
#2796 = CARTESIAN_POINT ( 'NONE',  ( 4.037591185471563371, -84.79547149457074795, 5.718994135553860936 ) ) ;
#2797 = CARTESIAN_POINT ( 'NONE',  ( -80.00000000000000000, -2.168404344971008868E-15, 12.50000000000000000 ) ) ;
#2798 =( BOUNDED_CURVE ( )  B_SPLINE_CURVE ( 2, ( #3583, #6109, #1015, #2490, #7626, #3792, #8140, #4291, #1861, #1820, #5595, #1140, #3665, #5051, #3119, #7670, #5674, #1180, #1734, #3625, #4372, #3033, #1054, #6192, #6863, #1223, #6233, #6947, #1093, #5637, #459, #418, #8177, #4328, #2406, #4967, #7543, #6364, #6322, #1773, #8256, #4409, #3748, #6902, #3709, #6279, #6991, #581, #4251, #3163, #541, #497, #2991, #3075, #8218, #2446, #5008, #7581, #5718, #8297, #5557, #2368, #7504, #4931, #2527, #5090, #6821, #4579, #7711, #3332, #3377, #7843, #2660, #3957, #3999, #663, #751, #6442, #5758, #7798, #5218, #7163, #795, #621, #2703, #3246, #1386, #1346, #6529, #4452, #5176, #706, #6485, #1432, #1903, #3290, #5802, #5890, #6403, #2030, #4622, #31, #5849, #2614, #120, #1261, #5262, #3917, #4558, #5936, #7755, #77, #164, #1987, #7033, #3833, #3202, #2571, #4537, #7118, #2070, #6569, #7207, #2744, #5305, #5132, #1944, #4497, #7076, #1303, #3873, #6769, #3455, #364, #3417, #2112, #6731, #6652, #2863, #6139, #1555, #7888, #3491, #3570, #2941, #4043, #5981, #1004, #881, #4120, #4666, #6019, #7247, #1473, #6610, #837, #7968, #243, #8008, #5426, #4836, #2823, #2236, #5387, #4080, #205, #6688, #2193, #3530, #2784, #5343, #7414, #7928, #919, #1595, #6062, #4745, #962, #7329, #2154, #286, #4708, #4792, #7366, #7286, #1512, #4160, #1639, #6098, #325, #2904, #5469, #8048, #2275, #4199, #5585, #1722, #8129, #5547, #5040, #7569, #1044, #2359, #3108, #3063, #6853, #2395, #4921, #3737, #4361, #569, #6935, #2435, #4955, #408, #7532, #1806, #2981, #3655, #3614, #6223, #1084, #4242, #486, #6811, #6890, #6307, #529, #446, #5663, #7493, #8166, #4280, #8089, #8244, #3023, #1682, #5624, #5508, #2477, #6182, #8205, #4997, #6976, #1763, #4318, #2316, #1848, #4880, #1124, #7613, #3698, #1169, #4398, #6268, #1211, #3781, #7452, #6351, #7021, #3941 ),
 .UNSPECIFIED., .F., .T. ) 
 B_SPLINE_CURVE_WITH_KNOTS ( ( 3, 2, 2, 2, 2, 2, 2, 2, 2, 2, 2, 2, 2, 2, 2, 2, 2, 2, 2, 2, 2, 2, 2, 2, 2, 2, 2, 2, 2, 2, 2, 2, 2, 2, 2, 2, 2, 2, 2, 2, 2, 2, 2, 2, 2, 2, 2, 2, 2, 2, 2, 2, 2, 2, 2, 2, 2, 2, 2, 2, 2, 2, 2, 2, 2, 2, 2, 2, 2, 2, 2, 2, 2, 2, 2, 2, 2, 2, 2, 2, 2, 2, 2, 2, 2, 2, 2, 2, 2, 2, 2, 2, 2, 2, 2, 2, 2, 2, 2, 2, 2, 2, 2, 2, 2, 2, 2, 2, 2, 2, 2, 2, 2, 2, 2, 2, 2, 2, 2, 2, 2, 2, 2, 2, 2, 2, 2, 2, 2, 2, 3 ),
 ( 0.000000000000000000, 0.007692307692307692735, 0.01538461538461538547, 0.02307692307692307820, 0.03076923076923077094, 0.03846153846153846367, 0.04615384615384615641, 0.05384615384615384914, 0.06153846153846154188, 0.06923076923076923461, 0.07692307692307692735, 0.08461538461538462008, 0.09230769230769231282, 0.1000000000000000056, 0.1076923076923076983, 0.1153846153846153910, 0.1230769230769230838, 0.1307692307692307765, 0.1384615384615384692, 0.1461538461538461620, 0.1538461538461538547, 0.1615384615384615474, 0.1692307692307692402, 0.1769230769230769329, 0.1846153846153846256, 0.1923076923076923184, 0.2000000000000000111, 0.2076923076923077038, 0.2153846153846153966, 0.2230769230769230893, 0.2307692307692307820, 0.2384615384615384748, 0.2461538461538461675, 0.2538461538461538325, 0.2615384615384615530, 0.2692307692307692180, 0.2769230769230769384, 0.2846153846153846034, 0.2923076923076923239, 0.2999999999999999889, 0.3076923076923077094, 0.3153846153846153744, 0.3230769230769230949, 0.3307692307692307598, 0.3384615384615384803, 0.3461538461538461453, 0.3538461538461538658, 0.3615384615384615308, 0.3692307692307692513, 0.3769230769230769162, 0.3846153846153846367, 0.3923076923076923017, 0.4000000000000000222, 0.4076923076923076872, 0.4153846153846154077, 0.4230769230769230727, 0.4307692307692307931, 0.4384615384615384581, 0.4461538461538461786, 0.4538461538461538436, 0.4615384615384615641, 0.4692307692307692291, 0.4769230769230769496, 0.4846153846153846145, 0.4923076923076923350, 0.5000000000000000000, 0.5076923076923076650, 0.5153846153846153300, 0.5230769230769231060, 0.5307692307692307709, 0.5384615384615384359, 0.5461538461538461009, 0.5538461538461538769, 0.5615384615384615419, 0.5692307692307692069, 0.5769230769230768718, 0.5846153846153846478, 0.5923076923076923128, 0.5999999999999999778, 0.6076923076923076428, 0.6153846153846154188, 0.6230769230769230838, 0.6307692307692307487, 0.6384615384615384137, 0.6461538461538461897, 0.6538461538461538547, 0.6615384615384615197, 0.6692307692307691847, 0.6769230769230769607, 0.6846153846153846256, 0.6923076923076922906, 0.6999999999999999556, 0.7076923076923077316, 0.7153846153846153966, 0.7230769230769230616, 0.7307692307692307265, 0.7384615384615385025, 0.7461538461538461675, 0.7538461538461538325, 0.7615384615384614975, 0.7692307692307692735, 0.7769230769230769384, 0.7846153846153846034, 0.7923076923076922684, 0.8000000000000000444, 0.8076923076923077094, 0.8153846153846153744, 0.8230769230769230393, 0.8307692307692308153, 0.8384615384615384803, 0.8461538461538461453, 0.8538461538461538103, 0.8615384615384615863, 0.8692307692307692513, 0.8769230769230769162, 0.8846153846153845812, 0.8923076923076923572, 0.9000000000000000222, 0.9076923076923076872, 0.9153846153846153522, 0.9230769230769231282, 0.9307692307692307931, 0.9384615384615384581, 0.9461538461538461231, 0.9538461538461538991, 0.9615384615384615641, 0.9692307692307692291, 0.9769230769230768940, 0.9846153846153846700, 0.9923076923076923350, 1.000000000000000000 ),
 .UNSPECIFIED. ) 
 CURVE ( )  GEOMETRIC_REPRESENTATION_ITEM ( )  RATIONAL_B_SPLINE_CURVE ( ( 1.000000000000000000, 0.9510565162951535312, 1.000000000000000000, 0.9510565162951535312, 1.000000000000000000, 0.9510565162951535312, 1.000000000000000000, 0.9510565162951535312, 1.000000000000000000, 0.9510565162951535312, 1.000000000000000000, 0.9510565162951535312, 1.000000000000000000, 0.9510565162951535312, 1.000000000000000000, 0.9510565162951535312, 1.000000000000000000, 0.9510565162951535312, 1.000000000000000000, 0.9510565162951535312, 1.000000000000000000, 0.9510565162951535312, 1.000000000000000000, 0.9510565162951535312, 1.000000000000000000, 0.9510565162951535312, 1.000000000000000000, 0.9510565162951535312, 1.000000000000000000, 0.9510565162951535312, 1.000000000000000000, 0.9510565162951535312, 1.000000000000000000, 0.9510565162951535312, 1.000000000000000000, 0.9510565162951535312, 1.000000000000000000, 0.9510565162951535312, 1.000000000000000000, 0.9510565162951535312, 1.000000000000000000, 0.9510565162951535312, 1.000000000000000000, 0.9510565162951535312, 1.000000000000000000, 0.9510565162951535312, 1.000000000000000000, 0.9510565162951535312, 1.000000000000000000, 0.9510565162951535312, 1.000000000000000000, 0.9510565162951535312, 1.000000000000000000, 0.9510565162951535312, 1.000000000000000000, 0.9510565162951535312, 1.000000000000000000, 0.9510565162951535312, 1.000000000000000000, 0.9510565162951535312, 1.000000000000000000, 0.9510565162951535312, 1.000000000000000000, 0.9510565162951535312, 1.000000000000000000, 0.9510565162951535312, 1.000000000000000000, 0.9510565162951535312, 1.000000000000000000, 0.9510565162951535312, 1.000000000000000000, 0.9510565162951535312, 1.000000000000000000, 0.9510565162951535312, 1.000000000000000000, 0.9510565162951535312, 1.000000000000000000, 0.9510565162951535312, 1.000000000000000000, 0.9510565162951535312, 1.000000000000000000, 0.9510565162951535312, 1.000000000000000000, 0.9510565162951535312, 1.000000000000000000, 0.9510565162951535312, 1.000000000000000000, 0.9510565162951535312, 1.000000000000000000, 0.9510565162951535312, 1.000000000000000000, 0.9510565162951535312, 1.000000000000000000, 0.9510565162951535312, 1.000000000000000000, 0.9510565162951535312, 1.000000000000000000, 0.9510565162951535312, 1.000000000000000000, 0.9510565162951535312, 1.000000000000000000, 0.9510565162951535312, 1.000000000000000000, 0.9510565162951535312, 1.000000000000000000, 0.9510565162951535312, 1.000000000000000000, 0.9510565162951535312, 1.000000000000000000, 0.9510565162951535312, 1.000000000000000000, 0.9510565162951535312, 1.000000000000000000, 0.9510565162951535312, 1.000000000000000000, 0.9510565162951535312, 1.000000000000000000, 0.9510565162951535312, 1.000000000000000000, 0.9510565162951535312, 1.000000000000000000, 0.9510565162951535312, 1.000000000000000000, 0.9510565162951535312, 1.000000000000000000, 0.9510565162951535312, 1.000000000000000000, 0.9510565162951535312, 1.000000000000000000, 0.9510565162951535312, 1.000000000000000000, 0.9510565162951535312, 1.000000000000000000, 0.9510565162951535312, 1.000000000000000000, 0.9510565162951535312, 1.000000000000000000, 0.9510565162951535312, 1.000000000000000000, 0.9510565162951535312, 1.000000000000000000, 0.9510565162951535312, 1.000000000000000000, 0.9510565162951535312, 1.000000000000000000, 0.9510565162951535312, 1.000000000000000000, 0.9510565162951535312, 1.000000000000000000, 0.9510565162951535312, 1.000000000000000000, 0.9510565162951535312, 1.000000000000000000, 0.9510565162951535312, 1.000000000000000000, 0.9510565162951535312, 1.000000000000000000, 0.9510565162951535312, 1.000000000000000000, 0.9510565162951535312, 1.000000000000000000, 0.9510565162951535312, 1.000000000000000000, 0.9510565162951535312, 1.000000000000000000, 0.9510565162951535312, 1.000000000000000000, 0.9510565162951535312, 1.000000000000000000, 0.9510565162951535312, 1.000000000000000000, 0.9510565162951535312, 1.000000000000000000, 0.9510565162951535312, 1.000000000000000000, 0.9510565162951535312, 1.000000000000000000, 0.9510565162951535312, 1.000000000000000000, 0.9510565162951535312, 1.000000000000000000, 0.9510565162951535312, 1.000000000000000000, 0.9510565162951535312, 1.000000000000000000, 0.9510565162951535312, 1.000000000000000000, 0.9510565162951535312, 1.000000000000000000, 0.9510565162951535312, 1.000000000000000000, 0.9510565162951535312, 1.000000000000000000, 0.9510565162951535312, 1.000000000000000000, 0.9510565162951535312, 1.000000000000000000, 0.9510565162951535312, 1.000000000000000000, 0.9510565162951535312, 1.000000000000000000, 0.9510565162951535312, 1.000000000000000000, 0.9510565162951535312, 1.000000000000000000, 0.9510565162951535312, 1.000000000000000000, 0.9510565162951535312, 1.000000000000000000, 0.9510565162951535312, 1.000000000000000000, 0.9510565162951535312, 1.000000000000000000, 0.9510565162951535312, 1.000000000000000000, 0.9510565162951535312, 1.000000000000000000, 0.9510565162951535312, 1.000000000000000000, 0.9510565162951535312, 1.000000000000000000, 0.9510565162951535312, 1.000000000000000000, 0.9510565162951535312, 1.000000000000000000, 0.9510565162951535312, 1.000000000000000000, 0.9510565162951535312, 1.000000000000000000, 0.9510565162951535312, 1.000000000000000000, 0.9510565162951535312, 1.000000000000000000, 0.9510565162951535312, 1.000000000000000000, 0.9510565162951535312, 1.000000000000000000, 0.9510565162951535312, 1.000000000000000000, 0.9510565162951535312, 1.000000000000000000, 0.9510565162951535312, 1.000000000000000000, 0.9510565162951535312, 1.000000000000000000, 0.9510565162951535312, 1.000000000000000000, 0.9510565162951535312, 1.000000000000000000, 0.9510565162951535312, 1.000000000000000000, 0.9510565162951535312, 1.000000000000000000, 0.9510565162951535312, 1.000000000000000000, 0.9510565162951535312, 1.000000000000000000, 0.9510565162951535312, 1.000000000000000000, 0.9510565162951535312, 1.000000000000000000 ) ) 
 REPRESENTATION_ITEM ( '' )  );
#2799 = LINE ( 'NONE', #3431, #7705 ) ;
#2800 = CARTESIAN_POINT ( 'NONE',  ( -2.823794231030041235, -68.59547149457073090, -1.017458915287723364 ) ) ;
#2801 = ORIENTED_EDGE ( 'NONE', *, *, #576, .F. ) ;
#2802 = CARTESIAN_POINT ( 'NONE',  ( 4.784657899331208775, -71.10452850542925773, 1.454677039711774533 ) ) ;
#2803 = CARTESIAN_POINT ( 'NONE',  ( -2.369498399071057193, -78.34547149457074511, 6.969112962950058332 ) ) ;
#2804 = ORIENTED_EDGE ( 'NONE', *, *, #602, .T. ) ;
#2805 = VECTOR ( 'NONE', #3237, 1000.000000000000000 ) ;
#2806 = CARTESIAN_POINT ( 'NONE',  ( -4.725907263620323207, -63.90452850542925489, 1.635492904037698647 ) ) ;
#2807 = DIRECTION ( 'NONE',  ( 1.000000000000000000, 0.000000000000000000, 0.000000000000000000 ) ) ;
#2808 = CARTESIAN_POINT ( 'NONE',  ( -4.312004677470993030, -75.04547149457074795, 3.009306630940933758 ) ) ;
#2809 = DIRECTION ( 'NONE',  ( -0.000000000000000000, 1.000000000000000000, 2.775557561562891351E-16 ) ) ;
#2810 = CARTESIAN_POINT ( 'NONE',  ( 4.312004677471013459, -97.54547149457070532, -3.009306630940933314 ) ) ;
#2811 = CARTESIAN_POINT ( 'NONE',  ( -4.191402346623180897, -63.30452850542926058, -5.607243785695311900 ) ) ;
#2812 = ORIENTED_EDGE ( 'NONE', *, *, #5575, .F. ) ;
#2813 = LINE ( 'NONE', #2143, #6116 ) ;
#2814 = CARTESIAN_POINT ( 'NONE',  ( -4.784657899331190123, -81.60452850542925773, -1.454677039711773867 ) ) ;
#2815 = CARTESIAN_POINT ( 'NONE',  ( 7.360235569667875843, -62.25452850542926342, -0.09995255151731691212 ) ) ;
#2816 = CARTESIAN_POINT ( 'NONE',  ( 3.154386672714808437, -73.24547149457075079, 0.09995255151720662534 ) ) ;
#2817 = ORIENTED_EDGE ( 'NONE', *, *, #280, .F. ) ;
#2818 = CARTESIAN_POINT ( 'NONE',  ( 63.45299461620744808, 100.0000000000000000, 7.500000000000000000 ) ) ;
#2819 = FACE_OUTER_BOUND ( 'NONE', #870, .T. ) ;
#2820 = CARTESIAN_POINT ( 'NONE',  ( -4.194503406049316929, -76.05452850542926058, 3.171033256558100533 ) ) ;
#2821 = EDGE_CURVE ( 'NONE', #1663, #5257, #8117, .T. ) ;
#2822 = VERTEX_POINT ( 'NONE', #7439 ) ;
#2823 = CARTESIAN_POINT ( 'NONE',  ( 1.529537955723689890, -71.85452850542925773, -5.030887037049978971 ) ) ;
#2824 = CARTESIAN_POINT ( 'NONE',  ( 0.09506052544077742139, -85.99547149457075079, -2.999999999999997780 ) ) ;
#2825 = CIRCLE ( 'NONE', #798, 1.500000000000001776 ) ;
#2826 = CARTESIAN_POINT ( 'NONE',  ( -5.257311121191321490, -95.74547149457072237, -0.09995255151718371311 ) ) ;
#2827 = CARTESIAN_POINT ( 'NONE',  ( -1.529537955723670795, -73.35452850542922931, 5.030887037049979860 ) ) ;
#2828 = CARTESIAN_POINT ( 'NONE',  ( -4.037591185471424815, -58.20452850542925916, 5.718994135553947977 ) ) ;
#2829 = CARTESIAN_POINT ( 'NONE',  ( 7.360235569667880284, -92.25452850542926342, -0.09995255151731691212 ) ) ;
#2830 = CARTESIAN_POINT ( 'NONE',  ( 1.840261337453269919, -67.80452850542926058, 2.371175808195547852 ) ) ;
#2831 = ORIENTED_EDGE ( 'NONE', *, *, #2789, .F. ) ;
#2832 = DIRECTION ( 'NONE',  ( 0.000000000000000000, 0.000000000000000000, 1.000000000000000000 ) ) ;
#2833 = VECTOR ( 'NONE', #2139, 1000.000000000000114 ) ;
#2834 = CARTESIAN_POINT ( 'NONE',  ( -80.00000000000000000, -25.00000000000000000, 20.00000000000000000 ) ) ;
#2835 = CARTESIAN_POINT ( 'NONE',  ( -2.493201789345251829, -76.05452850542926058, 1.934965279058294518 ) ) ;
#2836 = CARTESIAN_POINT ( 'NONE',  ( 4.191402346623198660, -91.80452850542926058, 5.607243785695311900 ) ) ;
#2837 = CARTESIAN_POINT ( 'NONE',  ( 0.09506052544073614885, -91.99547149457075079, -6.999999999999997335 ) ) ;
#2838 = DIRECTION ( 'NONE',  ( -1.000000000000000000, 0.000000000000000000, -0.000000000000000000 ) ) ;
#2839 = CARTESIAN_POINT ( 'NONE',  ( -80.00000000000000000, 0.000000000000000000, -20.00000000000000000 ) ) ;
#2840 = AXIS2_PLACEMENT_3D ( 'NONE', #8120, #5497, #1756 ) ;
#2841 = CARTESIAN_POINT ( 'NONE',  ( 2.610703060766943029, -64.54547149457073374, -1.773238653441125523 ) ) ;
#2842 = UNCERTAINTY_MEASURE_WITH_UNIT (LENGTH_MEASURE( 1.000000000000000082E-05 ), #6571, 'distance_accuracy_value', 'NONE');
#2843 = FILL_AREA_STYLE ('',( #4810 ) ) ;
#2844 = ORIENTED_EDGE ( 'NONE', *, *, #7496, .F. ) ;
#2845 = CARTESIAN_POINT ( 'NONE',  ( -1.529537955723671683, -64.35452850542924352, 5.030887037049979860 ) ) ;
#2846 = CARTESIAN_POINT ( 'NONE',  ( -4.037591185471543831, -83.29547149457074795, -5.718994135553860936 ) ) ;
#2847 = DIRECTION ( 'NONE',  ( -0.000000000000000000, -0.000000000000000000, 1.000000000000000000 ) ) ;
#2848 = CARTESIAN_POINT ( 'NONE',  ( 1.719659006605285478, -73.84547149457074511, -4.969112962950050338 ) ) ;
#2849 = CARTESIAN_POINT ( 'NONE',  ( -4.194503406049319594, -70.05452850542923215, 3.171033256558100533 ) ) ;
#2850 = CARTESIAN_POINT ( 'NONE',  ( 0.000000000000000000, 0.000000000000000000, 7.500000000000000000 ) ) ;
#2851 = CARTESIAN_POINT ( 'NONE',  ( -1.529537955723777820, -71.14547149457071384, -5.030887037049945221 ) ) ;
#2852 = DIRECTION ( 'NONE',  ( 0.000000000000000000, -1.734723475976807094E-16, 1.000000000000000000 ) ) ;
#2853 = CARTESIAN_POINT ( 'NONE',  ( -5.257311121191321490, -95.74547149457072237, -0.09995255151718371311 ) ) ;
#2854 = CARTESIAN_POINT ( 'NONE',  ( 6.628020296210639373, -59.40452850542925489, -2.253526892787612645 ) ) ;
#2855 = VERTEX_POINT ( 'NONE', #5614 ) ;
#2856 = ADVANCED_FACE ( 'NONE', ( #4986 ), #5457, .F. ) ;
#2857 = CARTESIAN_POINT ( 'NONE',  ( 2.862020680886514956, -80.70452850542925205, -4.100960146804039752 ) ) ;
#2858 = VERTEX_POINT ( 'NONE', #8036 ) ;
#2859 = CARTESIAN_POINT ( 'NONE',  ( -80.00000000000000000, -19.99999999999999645, -12.50000000000000355 ) ) ;
#2860 = CARTESIAN_POINT ( 'NONE',  ( -0.09506052544083884448, -87.00452850542924921, -4.999999999999997335 ) ) ;
#2861 = CARTESIAN_POINT ( 'NONE',  ( -0.09506052544083960776, -81.00452850542926342, -4.999999999999997335 ) ) ;
#2862 = VERTEX_POINT ( 'NONE', #6880 ) ;
#2863 = CARTESIAN_POINT ( 'NONE',  ( -3.015831842038215083, -75.30452850542926058, -3.989209796945429432 ) ) ;
#2864 = CARTESIAN_POINT ( 'NONE',  ( -2.823794231030039903, -80.59547149457075932, -1.017458915287723364 ) ) ;
#2865 = CARTESIAN_POINT ( 'NONE',  ( -2.823794231030042567, -59.59547149457074511, -1.017458915287723364 ) ) ;
#2866 = CARTESIAN_POINT ( 'NONE',  ( 5.257311121191341918, -74.25452850542924921, -0.09995255151729465215 ) ) ;
#2867 = CARTESIAN_POINT ( 'NONE',  ( -6.628020296210620721, -84.90452850542926910, 2.253526892787613978 ) ) ;
#2868 = CARTESIAN_POINT ( 'NONE',  ( -1.069819614139540409, -60.15452850542926200, -2.969112962950023249 ) ) ;
#2869 = AXIS2_PLACEMENT_3D ( 'NONE', #4595, #7771, #2126 ) ;
#2870 = EDGE_LOOP ( 'NONE', ( #3399, #1717 ) ) ;
#2871 = CARTESIAN_POINT ( 'NONE',  ( 75.00000000000000000, -9.999999999999994671, 0.000000000000000000 ) ) ;
#2872 = DIRECTION ( 'NONE',  ( 0.000000000000000000, 0.000000000000000000, -1.000000000000000000 ) ) ;
#2873 = CARTESIAN_POINT ( 'NONE',  ( -1.069819614139537967, -81.15452850542924068, -2.969112962950023249 ) ) ;
#2874 = CARTESIAN_POINT ( 'NONE',  ( -2.179377348189460051, -85.35452850542924352, 7.030887037049988741 ) ) ;
#2875 = CARTESIAN_POINT ( 'NONE',  ( 4.037591185471562483, -78.79547149457074795, 5.718994135553860936 ) ) ;
#2876 = DIRECTION ( 'NONE',  ( 0.000000000000000000, 2.168404344971010347E-16, -1.000000000000000000 ) ) ;
#2877 = LINE ( 'NONE', #6702, #6242 ) ;
#2878 = CARTESIAN_POINT ( 'NONE',  ( -2.823794231030020363, -81.90452850542925489, 1.017458915287783316 ) ) ;
#2879 = COLOUR_RGB ( '', 0.72549020, 0.75294118, 0.79215686) ;
#2880 = VECTOR ( 'NONE', #6606, 1000.000000000000000 ) ;
#2881 = ORIENTED_EDGE ( 'NONE', *, *, #7035, .F. ) ;
#2882 = CARTESIAN_POINT ( 'NONE',  ( -0.9662349396012467340, -27.25766265056033433, 4.500000000000000888 ) ) ;
#2883 = CARTESIAN_POINT ( 'NONE',  ( -4.784657899331191899, -63.60452850542925063, -1.454677039711773867 ) ) ;
#2884 = CARTESIAN_POINT ( 'NONE',  ( 7.360235569667878508, -82.24547149457073658, 0.09995255151716216091 ) ) ;
#2885 = ORIENTED_EDGE ( 'NONE', *, *, #12, .T. ) ;
#2886 = CARTESIAN_POINT ( 'NONE',  ( -0.09506052544073541333, -75.49547149457073658, 4.999999999999997335 ) ) ;
#2887 = CARTESIAN_POINT ( 'NONE',  ( 3.015831842038148025, -70.69547149457073942, -3.989209796945492048 ) ) ;
#2888 = VECTOR ( 'NONE', #7689, 1000.000000000000114 ) ;
#2889 = CARTESIAN_POINT ( 'NONE',  ( 4.725907263620340082, -65.40452850542925489, -1.635492904037697981 ) ) ;
#2890 = ADVANCED_BREP_SHAPE_REPRESENTATION ( '', ( #4458, #2840 ), #2157 ) ;
#2891 = CARTESIAN_POINT ( 'NONE',  ( 1.097606853890779561E-14, -87.00000000000001421, 0.000000000000000000 ) ) ;
#2892 = MECHANICAL_DESIGN_GEOMETRIC_PRESENTATION_REPRESENTATION (  '', ( #8272 ), #3693 ) ;
#2893 = CARTESIAN_POINT ( 'NONE',  ( -2.862020680886581570, -68.29547149457074795, -4.100960146803977580 ) ) ;
#2894 = CARTESIAN_POINT ( 'NONE',  ( 54.99999999999999289, -30.00000000000000000, 7.499999999999992006 ) ) ;
#2895 = CARTESIAN_POINT ( 'NONE',  ( -6.013306294175153610, -63.45452850542924494, -4.245374608440613429 ) ) ;
#2896 = ORIENTED_EDGE ( 'NONE', *, *, #7440, .F. ) ;
#2897 = FACE_OUTER_BOUND ( 'NONE', #2937, .T. ) ;
#2898 = EDGE_CURVE ( 'NONE', #5070, #3497, #4230, .T. ) ;
#2899 = EDGE_LOOP ( 'NONE', ( #7653, #5976, #3115, #7242 ) ) ;
#2900 = CARTESIAN_POINT ( 'NONE',  ( -65.00000000000000000, -12.00000000000000355, -12.50000000000000178 ) ) ;
#2901 = CARTESIAN_POINT ( 'NONE',  ( 2.862020680886515844, -89.70452850542926626, -4.100960146804039752 ) ) ;
#2902 = CARTESIAN_POINT ( 'NONE',  ( 4.784657899331210551, -83.10452850542927195, 1.454677039711774533 ) ) ;
#2903 = ORIENTED_EDGE ( 'NONE', *, *, #3156, .T. ) ;
#2904 = CARTESIAN_POINT ( 'NONE',  ( 0.09506052544085895339, -67.50452850542926342, 4.999999999999997335 ) ) ;
#2905 = CARTESIAN_POINT ( 'NONE',  ( -1.069819614139473796, -84.34547149457075932, 2.969112962950044121 ) ) ;
#2906 = CARTESIAN_POINT ( 'NONE',  ( 4.725907263620374721, -94.09547149457074511, 1.635492904037598283 ) ) ;
#2907 = CARTESIAN_POINT ( 'NONE',  ( -4.725907263620321430, -72.90452850542925489, 1.635492904037698647 ) ) ;
#2908 = CARTESIAN_POINT ( 'NONE',  ( -4.037591185471422150, -85.20452850542925205, 5.718994135553947977 ) ) ;
#2909 = CARTESIAN_POINT ( 'NONE',  ( -2.823794231030023472, -57.90452850542925489, 1.017458915287783316 ) ) ;
#2910 = VERTEX_POINT ( 'NONE', #6168 ) ;
#2911 = DIRECTION ( 'NONE',  ( 1.000000000000000000, 0.000000000000000000, 0.000000000000000000 ) ) ;
#2912 = DIRECTION ( 'NONE',  ( 1.000000000000000000, 0.000000000000000000, 0.000000000000000000 ) ) ;
#2913 = CARTESIAN_POINT ( 'NONE',  ( -1.840261337453252821, -69.30452850542926058, -2.371175808195547852 ) ) ;
#2914 = CARTESIAN_POINT ( 'NONE',  ( 2.369498399071225503, -79.65452850542925489, 6.969112962950009482 ) ) ;
#2915 = CARTESIAN_POINT ( 'NONE',  ( 6.628020296210687334, -79.09547149457075932, 2.253526892787472757 ) ) ;
#2916 = CARTESIAN_POINT ( 'NONE',  ( 54.99999999999999289, -30.00000000000000000, -7.500000000000007105 ) ) ;
#2917 = CARTESIAN_POINT ( 'NONE',  ( -1.719659006605263718, -93.34547149457073090, 4.969112962950051227 ) ) ;
#2918 = CARTESIAN_POINT ( 'NONE',  ( -1.069819614139537522, -84.15452850542925489, -2.969112962950023249 ) ) ;
#2919 = EDGE_CURVE ( 'NONE', #4993, #1241, #1111, .T. ) ;
#2920 = UNCERTAINTY_MEASURE_WITH_UNIT (LENGTH_MEASURE( 1.000000000000000082E-05 ), #1366, 'distance_accuracy_value', 'NONE');
#2921 = SURFACE_SIDE_STYLE ('',( #7945 ) ) ;
#2922 = ORIENTED_EDGE ( 'NONE', *, *, #3935, .T. ) ;
#2923 = DIRECTION ( 'NONE',  ( 1.000000000000000000, 0.000000000000000000, 0.000000000000000000 ) ) ;
#2924 = CARTESIAN_POINT ( 'NONE',  ( 4.784657899331207886, -62.10452850542925063, 1.454677039711774533 ) ) ;
#2925 = CARTESIAN_POINT ( 'NONE',  ( 4.037591185471562483, -78.79547149457074795, 5.718994135553860936 ) ) ;
#2926 = ORIENTED_EDGE ( 'NONE', *, *, #3884, .F. ) ;
#2927 = CARTESIAN_POINT ( 'NONE',  ( -1.719659006605266383, -72.34547149457073090, 4.969112962950051227 ) ) ;
#2928 = CARTESIAN_POINT ( 'NONE',  ( -4.194503406049384431, -71.44547149457075363, -3.171033256558012159 ) ) ;
#2929 = CARTESIAN_POINT ( 'NONE',  ( 2.862020680886512292, -62.70452850542926626, -4.100960146804039752 ) ) ;
#2930 = CARTESIAN_POINT ( 'NONE',  ( 55.00000000000002132, -99.99999999999998579, -20.00000000000000000 ) ) ;
#2931 = CARTESIAN_POINT ( 'NONE',  ( 4.784657899331176800, -67.39547149457074227, -1.454677039711874009 ) ) ;
#2932 = VECTOR ( 'NONE', #2291, 1000.000000000000000 ) ;
#2933 = FILL_AREA_STYLE ('',( #7443 ) ) ;
#2934 = CARTESIAN_POINT ( 'NONE',  ( -7.360235569667860744, -63.75452850542926342, 0.09995255151731782806 ) ) ;
#2935 = ORIENTED_EDGE ( 'NONE', *, *, #2287, .T. ) ;
#2936 = PLANE ( 'NONE',  #3559 ) ;
#2937 = EDGE_LOOP ( 'NONE', ( #6441, #2935, #4800, #316 ) ) ;
#2938 = PLANE ( 'NONE',  #6906 ) ;
#2939 = CARTESIAN_POINT ( 'NONE',  ( 4.784657899331210551, -83.10452850542927195, 1.454677039711774533 ) ) ;
#2940 = CARTESIAN_POINT ( 'NONE',  ( 5.257311121191341918, -74.25452850542924921, -0.09995255151729465215 ) ) ;
#2941 = CARTESIAN_POINT ( 'NONE',  ( 4.725907263620340082, -74.40452850542925489, -1.635492904037697981 ) ) ;
#2942 = CARTESIAN_POINT ( 'NONE',  ( -2.610703060766925709, -81.04547149457074795, 1.773238653441125745 ) ) ;
#2943 = CARTESIAN_POINT ( 'NONE',  ( -0.09506052544073276267, -96.49547149457075079, 4.999999999999997335 ) ) ;
#2944 = CARTESIAN_POINT ( 'NONE',  ( -0.09506052544084110656, -69.00452850542926342, -4.999999999999997335 ) ) ;
#2945 = CARTESIAN_POINT ( 'NONE',  ( -4.191402346623177344, -87.30452850542926058, -5.607243785695311900 ) ) ;
#2946 = CARTESIAN_POINT ( 'NONE',  ( -1.686450176301568016, -58.20452850542925916, 2.482926158054133303 ) ) ;
#2947 = VECTOR ( 'NONE', #8056, 1000.000000000000000 ) ;
#2948 = SHAPE_DEFINITION_REPRESENTATION ( #3596, #7093 ) ;
#2949 = ORIENTED_EDGE ( 'NONE', *, *, #102, .F. ) ;
#2950 = FACE_OUTER_BOUND ( 'NONE', #7388, .T. ) ;
#2951 = ORIENTED_EDGE ( 'NONE', *, *, #52, .F. ) ;
#2952 = DIRECTION ( 'NONE',  ( 0.000000000000000000, -0.000000000000000000, -1.000000000000000000 ) ) ;
#2953 = CARTESIAN_POINT ( 'NONE',  ( -2.823794231030022139, -69.90452850542925489, 1.017458915287783316 ) ) ;
#2954 = VECTOR ( 'NONE', #6953, 1000.000000000000000 ) ;
#2955 = CARTESIAN_POINT ( 'NONE',  ( -4.191402346623058328, -78.19547149457073942, 5.607243785695398941 ) ) ;
#2956 = LINE ( 'NONE', #4763, #6693 ) ;
#2957 = EDGE_CURVE ( 'NONE', #1136, #1530, #4147, .T. ) ;
#2958 = CARTESIAN_POINT ( 'NONE',  ( 4.302742873392585210, -96.99999999999947420, 2.548615363087012753 ) ) ;
#2959 = CARTESIAN_POINT ( 'NONE',  ( -1.840261337453250823, -84.30452850542926058, -2.371175808195547852 ) ) ;
#2960 = EDGE_CURVE ( 'NONE', #5449, #6860, #4819, .T. ) ;
#2961 = VECTOR ( 'NONE', #1585, 1000.000000000000000 ) ;
#2962 = VERTEX_POINT ( 'NONE', #1031 ) ;
#2963 = DIRECTION ( 'NONE',  ( 0.000000000000000000, 0.000000000000000000, 1.000000000000000000 ) ) ;
#2964 = CARTESIAN_POINT ( 'NONE',  ( 2.862020680886511848, -59.70452850542925205, -4.100960146804039752 ) ) ;
#2965 = CARTESIAN_POINT ( 'NONE',  ( 5.895805022753492608, -72.94547149457073942, 4.407101234057782868 ) ) ;
#2966 = VERTEX_POINT ( 'NONE', #2930 ) ;
#2967 = CARTESIAN_POINT ( 'NONE',  ( -4.194503406049383543, -71.44547149457073942, -3.171033256558012159 ) ) ;
#2968 = CARTESIAN_POINT ( 'NONE',  ( -1.719659006605265716, -72.34547149457071669, 4.969112962950051227 ) ) ;
#2969 = CARTESIAN_POINT ( 'NONE',  ( 1.529537955723688780, -62.85452850542925063, -5.030887037049978971 ) ) ;
#2970 = PLANE ( 'NONE',  #4352 ) ;
#2971 = CARTESIAN_POINT ( 'NONE',  ( 4.194503406049400418, -60.94547149457072521, 3.171033256558012159 ) ) ;
#2972 =( LENGTH_UNIT ( ) NAMED_UNIT ( * ) SI_UNIT ( .MILLI., .METRE. ) );
#2973 = CARTESIAN_POINT ( 'NONE',  ( 3.015831842038236399, -94.80452850542924637, 3.989209796945429432 ) ) ;
#2974 = VERTEX_POINT ( 'NONE', #6758 ) ;
#2975 = CARTESIAN_POINT ( 'NONE',  ( -1.500000000000001332, -27.00000000000000000, 4.500000000000000888 ) ) ;
#2976 = EDGE_CURVE ( 'NONE', #2259, #1658, #5695, .T. ) ;
#2977 = EDGE_LOOP ( 'NONE', ( #4835, #6883, #3718, #3019 ) ) ;
#2978 = LINE ( 'NONE', #6850, #3812 ) ;
#2979 = CARTESIAN_POINT ( 'NONE',  ( 1.719659006605391616, -82.65452850542925489, 4.969112962950016588 ) ) ;
#2980 = CARTESIAN_POINT ( 'NONE',  ( -4.725907263620351628, -92.59547149457074511, -1.635492904037597617 ) ) ;
#2981 = CARTESIAN_POINT ( 'NONE',  ( -4.312004677471058756, -63.45452850542926626, -3.009306630940843608 ) ) ;
#2982 = CARTESIAN_POINT ( 'NONE',  ( 1.686450176301636850, -84.79547149457074795, 2.482926158054096000 ) ) ;
#2983 = CARTESIAN_POINT ( 'NONE',  ( 4.725907263620375609, -97.09547149457074511, 1.635492904037598283 ) ) ;
#2984 = CARTESIAN_POINT ( 'NONE',  ( -1.529537955723671683, -67.35452850542925773, 5.030887037049979860 ) ) ;
#2985 = CARTESIAN_POINT ( 'NONE',  ( 5.895805022753406455, -83.55452850542926058, -4.407101234057908989 ) ) ;
#2986 = CARTESIAN_POINT ( 'NONE',  ( 2.823794231030062551, -97.09547149457074511, 1.017458915287723809 ) ) ;
#2987 = SHAPE_DEFINITION_REPRESENTATION ( #7502, #4188 ) ;
#2988 = ORIENTED_EDGE ( 'NONE', *, *, #1570, .F. ) ;
#2989 = LINE ( 'NONE', #3031, #7659 ) ;
#2990 = ORIENTED_EDGE ( 'NONE', *, *, #7078, .T. ) ;
#2991 = CARTESIAN_POINT ( 'NONE',  ( -2.862020680886492752, -88.20452850542925205, 4.100960146804039752 ) ) ;
#2992 = CARTESIAN_POINT ( 'NONE',  ( 2.823794231030039015, -65.40452850542925489, -1.017458915287783316 ) ) ;
#2993 = CARTESIAN_POINT ( 'NONE',  ( -0.09506052544071416643, -75.49547149457075079, 6.999999999999997335 ) ) ;
#2994 = DIRECTION ( 'NONE',  ( 0.000000000000000000, 0.000000000000000000, 1.000000000000000000 ) ) ;
#2995 = VECTOR ( 'NONE', #2002, 1000.000000000000000 ) ;
#2996 = CARTESIAN_POINT ( 'NONE',  ( 0.09506052544075714594, -91.99547149457073658, -4.999999999999997335 ) ) ;
#2997 = CARTESIAN_POINT ( 'NONE',  ( 1.069819614139557729, -82.65452850542926910, 2.969112962950023249 ) ) ;
#2998 = SURFACE_STYLE_USAGE ( .BOTH. , #6913 ) ;
#2999 = EDGE_LOOP ( 'NONE', ( #7017, #1200, #3245, #3998 ) ) ;
#3000 = CARTESIAN_POINT ( 'NONE',  ( 55.00000000000000000, -25.00000000000002132, 20.00000000000000000 ) ) ;
#3001 = CARTESIAN_POINT ( 'NONE',  ( 4.312004677471073855, -61.95452850542923784, 3.009306630940844496 ) ) ;
#3002 = CARTESIAN_POINT ( 'NONE',  ( -2.369498399071057637, -75.34547149457073090, 6.969112962950058332 ) ) ;
#3003 = CARTESIAN_POINT ( 'NONE',  ( 4.331153185401124261, -96.99999999999995737, 2.564721935162156630 ) ) ;
#3004 = EDGE_CURVE ( 'NONE', #210, #7949, #3052, .T. ) ;
#3005 = CARTESIAN_POINT ( 'NONE',  ( 4.725907263620372945, -79.09547149457074511, 1.635492904037598283 ) ) ;
#3006 = CARTESIAN_POINT ( 'NONE',  ( 2.862020680886599333, -72.79547149457074795, 4.100960146803977580 ) ) ;
#3007 = CARTESIAN_POINT ( 'NONE',  ( 5.257311121191341918, -59.25452850542924210, -0.09995255151729465215 ) ) ;
#3008 = DIRECTION ( 'NONE',  ( -1.000000000000000000, 0.000000000000000000, -0.000000000000000000 ) ) ;
#3009 = AXIS2_PLACEMENT_3D ( 'NONE', #6469, #7780, #1286 ) ;
#3010 = CARTESIAN_POINT ( 'NONE',  ( 1.719659006605389617, -67.65452850542925489, 4.969112962950016588 ) ) ;
#3011 = EDGE_CURVE ( 'NONE', #540, #1594, #998, .T. ) ;
#3012 = CARTESIAN_POINT ( 'NONE',  ( 0.09506052544075374588, -64.99547149457075079, -4.999999999999997335 ) ) ;
#3013 = CARTESIAN_POINT ( 'NONE',  ( 1.529537955723692555, -92.85452850542925773, -5.030887037049978971 ) ) ;
#3014 = ORIENTED_EDGE ( 'NONE', *, *, #6561, .F. ) ;
#3015 = VECTOR ( 'NONE', #7593, 1000.000000000000000 ) ;
#3016 = UNCERTAINTY_MEASURE_WITH_UNIT (LENGTH_MEASURE( 1.000000000000000082E-05 ), #7238, 'distance_accuracy_value', 'NONE');
#3017 = FACE_OUTER_BOUND ( 'NONE', #6625, .T. ) ;
#3018 = CIRCLE ( 'NONE', #1539, 5.000000000000000888 ) ;
#3019 = ORIENTED_EDGE ( 'NONE', *, *, #7634, .T. ) ;
#3020 = CARTESIAN_POINT ( 'NONE',  ( -1.500000000000001110, -27.00000000000000000, -5.000000000000000000 ) ) ;
#3021 = CARTESIAN_POINT ( 'NONE',  ( 4.784657899331211439, -89.10452850542925773, 1.454677039711774533 ) ) ;
#3022 = CARTESIAN_POINT ( 'NONE',  ( -0.09506052544073390065, -87.49547149457075079, 4.999999999999997335 ) ) ;
#3023 = CARTESIAN_POINT ( 'NONE',  ( -5.257311121191325043, -60.75452850542925631, 0.09995255151729529053 ) ) ;
#3024 = CARTESIAN_POINT ( 'NONE',  ( -1.840261337453200197, -78.19547149457073942, 2.371175808195584267 ) ) ;
#3025 = CARTESIAN_POINT ( 'NONE',  ( 1.719659006605286811, -88.84547149457070248, -4.969112962950050338 ) ) ;
#3026 = CARTESIAN_POINT ( 'NONE',  ( 5.257311121191341918, -65.25452850542926342, -0.09995255151729465215 ) ) ;
#3027 = CARTESIAN_POINT ( 'NONE',  ( -0.09506052544086102118, -78.00452850542926342, -6.999999999999997335 ) ) ;
#3028 = CARTESIAN_POINT ( 'NONE',  ( -1.069819614139541075, -57.15452850542926200, -2.969112962950023249 ) ) ;
#3029 = ORIENTED_EDGE ( 'NONE', *, *, #508, .T. ) ;
#3030 = APPLICATION_CONTEXT ( 'automotive_design' ) ;
#3031 = CARTESIAN_POINT ( 'NONE',  ( -80.00000000000000000, -19.99999999999999645, -12.50000000000000355 ) ) ;
#3032 = ORIENTED_EDGE ( 'NONE', *, *, #4118, .T. ) ;
#3033 = CARTESIAN_POINT ( 'NONE',  ( 1.529537955723692555, -92.85452850542925773, -5.030887037049978971 ) ) ;
#3034 = CARTESIAN_POINT ( 'NONE',  ( 1.069819614139555952, -67.65452850542925489, 2.969112962950023249 ) ) ;
#3035 = CARTESIAN_POINT ( 'NONE',  ( 4.725907263620342746, -95.40452850542925489, -1.635492904037697981 ) ) ;
#3036 = CARTESIAN_POINT ( 'NONE',  ( 4.191402346623078756, -79.69547149457075363, -5.607243785695398941 ) ) ;
#3037 = CARTESIAN_POINT ( 'NONE',  ( 1.529537955723692999, -95.85452850542922931, -5.030887037049978971 ) ) ;
#3038 = ADVANCED_FACE ( 'NONE', ( #352, #5495 ), #2970, .F. ) ;
#3039 = CARTESIAN_POINT ( 'NONE',  ( -2.862020680886579793, -83.29547149457074795, -4.100960146803977580 ) ) ;
#3040 = CARTESIAN_POINT ( 'NONE',  ( 1.840261337453271917, -85.80452850542926058, 2.371175808195547852 ) ) ;
#3041 = DIRECTION ( 'NONE',  ( -0.000000000000000000, -0.000000000000000000, -1.000000000000000000 ) ) ;
#3042 = EDGE_LOOP ( 'NONE', ( #6591, #5673, #3523, #2270 ) ) ;
#3043 = EDGE_CURVE ( 'NONE', #2779, #8159, #476, .T. ) ;
#3044 = CARTESIAN_POINT ( 'NONE',  ( 47.49999999999998579, -88.00000000000000000, 0.000000000000000000 ) ) ;
#3045 = CARTESIAN_POINT ( 'NONE',  ( 2.862020680886512292, -62.70452850542926626, -4.100960146804039752 ) ) ;
#3046 = CARTESIAN_POINT ( 'NONE',  ( -4.037591185471544719, -74.29547149457074795, -5.718994135553860936 ) ) ;
#3047 = FILL_AREA_STYLE_COLOUR ( '', #6324 ) ;
#3048 = LINE ( 'NONE', #2419, #655 ) ;
#3049 = CARTESIAN_POINT ( 'NONE',  ( 4.725907263620372056, -70.09547149457074511, 1.635492904037598283 ) ) ;
#3050 = CARTESIAN_POINT ( 'NONE',  ( 2.862020680886598889, -69.79547149457074795, 4.100960146803977580 ) ) ;
#3051 = CARTESIAN_POINT ( 'NONE',  ( 0.09506052544085781542, -58.50452850542925631, 4.999999999999997335 ) ) ;
#3052 = LINE ( 'NONE', #6127, #7320 ) ;
#3053 = CARTESIAN_POINT ( 'NONE',  ( -4.312004677471058756, -66.45452850542925205, -3.009306630940844052 ) ) ;
#3054 = CARTESIAN_POINT ( 'NONE',  ( -4.784657899331159925, -62.89547149457074227, 1.454677039711874675 ) ) ;
#3055 = EDGE_LOOP ( 'NONE', ( #2111, #7565, #4948, #332, #7058 ) ) ;
#3056 = CARTESIAN_POINT ( 'NONE',  ( 50.00000000000000000, -19.99999999999999645, -12.50000000000000355 ) ) ;
#3057 = ADVANCED_FACE ( 'NONE', ( #7482 ), #2423, .F. ) ;
#3058 = VECTOR ( 'NONE', #4488, 1000.000000000000000 ) ;
#3059 = ORIENTED_EDGE ( 'NONE', *, *, #2117, .F. ) ;
#3060 = DIRECTION ( 'NONE',  ( 1.000000000000000000, -8.326672684688674053E-16, 0.000000000000000000 ) ) ;
#3061 = CARTESIAN_POINT ( 'NONE',  ( -5.257311121191324155, -75.75452850542922079, 0.09995255151729526277 ) ) ;
#3062 = CARTESIAN_POINT ( 'NONE',  ( 0.09506052544075714594, -91.99547149457073658, -4.999999999999997335 ) ) ;
#3063 = CARTESIAN_POINT ( 'NONE',  ( 4.725907263620340082, -65.40452850542925489, -1.635492904037697981 ) ) ;
#3064 = CARTESIAN_POINT ( 'NONE',  ( 1.686450176301635961, -75.79547149457074795, 2.482926158054096000 ) ) ;
#3065 = CARTESIAN_POINT ( 'NONE',  ( -7.360235569667858080, -81.75452850542926342, 0.09995255151731782806 ) ) ;
#3066 = CARTESIAN_POINT ( 'NONE',  ( -4.312004677470992142, -87.04547149457074795, 3.009306630940933758 ) ) ;
#3067 = CARTESIAN_POINT ( 'NONE',  ( -3.015831842038215971, -69.30452850542926058, -3.989209796945429432 ) ) ;
#3068 = CARTESIAN_POINT ( 'NONE',  ( -0.09506052544086064648, -81.00452850542926342, -6.999999999999997335 ) ) ;
#3069 = CARTESIAN_POINT ( 'NONE',  ( 3.154386672714811102, -91.24547149457073658, 0.09995255151720662534 ) ) ;
#3070 = EDGE_CURVE ( 'NONE', #8322, #293, #5574, .T. ) ;
#3071 = ORIENTED_EDGE ( 'NONE', *, *, #5463, .T. ) ;
#3072 = CARTESIAN_POINT ( 'NONE',  ( 43.45299461620743386, -9.999999999999994671, 0.000000000000000000 ) ) ;
#3073 = CARTESIAN_POINT ( 'NONE',  ( -0.09506052544073731458, -60.49547149457074369, 4.999999999999997335 ) ) ;
#3074 = EDGE_LOOP ( 'NONE', ( #114, #4062, #4119, #3349 ) ) ;
#3075 = CARTESIAN_POINT ( 'NONE',  ( -4.194503406049316041, -88.05452850542924637, 3.171033256558101865 ) ) ;
#3076 = CARTESIAN_POINT ( 'NONE',  ( -1.069819614139539521, -66.15452850542925489, -2.969112962950023249 ) ) ;
#3077 = CARTESIAN_POINT ( 'NONE',  ( -2.369498399071207739, -57.15452850542926200, -6.969112962950009482 ) ) ;
#3078 = CARTESIAN_POINT ( 'NONE',  ( -0.09506052544071491583, -69.49547149457075079, 6.999999999999997335 ) ) ;
#3079 = AXIS2_PLACEMENT_3D ( 'NONE', #969, #8017, #211 ) ;
#3080 = CARTESIAN_POINT ( 'NONE',  ( 5.257311121191342806, -82.24547149457073658, 0.09995255151718437925 ) ) ;
#3081 = CARTESIAN_POINT ( 'NONE',  ( -2.882544866740877065, -78.60452850542927195, -0.8366430509618996147 ) ) ;
#3082 =( NAMED_UNIT ( * ) SI_UNIT ( $, .STERADIAN. ) SOLID_ANGLE_UNIT ( ) );
#3083 = ORIENTED_EDGE ( 'NONE', *, *, #2344, .T. ) ;
#3084 = CARTESIAN_POINT ( 'NONE',  ( -5.257311121191324155, -57.75452850542923500, 0.09995255151729526277 ) ) ;
#3085 = CIRCLE ( 'NONE', #7803, 1.500000000000001332 ) ;
#3086 = VECTOR ( 'NONE', #7916, 1000.000000000000000 ) ;
#3087 = CARTESIAN_POINT ( 'NONE',  ( -5.895805022753477509, -74.44547149457072521, -4.407101234057782868 ) ) ;
#3088 = PRESENTATION_STYLE_ASSIGNMENT (( #985 ) ) ;
#3089 = CARTESIAN_POINT ( 'NONE',  ( 4.919969012183922352, -96.99999999999991473, -3.234920223772670411 ) ) ;
#3090 = CARTESIAN_POINT ( 'NONE',  ( 5.257311121191341030, -64.24547149457075079, 0.09995255151718437925 ) ) ;
#3091 = CARTESIAN_POINT ( 'NONE',  ( 4.037591185471564259, -93.79547149457076216, 5.718994135553860936 ) ) ;
#3092 = CARTESIAN_POINT ( 'NONE',  ( 2.823794231030042567, -92.40452850542925489, -1.017458915287783316 ) ) ;
#3093 = DIRECTION ( 'NONE',  ( 0.000000000000000000, 0.000000000000000000, -1.000000000000000000 ) ) ;
#3094 = AXIS2_PLACEMENT_3D ( 'NONE', #4624, #7209, #1434 ) ;
#3095 = ADVANCED_BREP_SHAPE_REPRESENTATION ( '', ( #4543, #2840 ), #7820 ) ;
#3096 = CARTESIAN_POINT ( 'NONE',  ( 4.312004677471073855, -64.95452850542926626, 3.009306630940844496 ) ) ;
#3097 = VECTOR ( 'NONE', #6576, 1000.000000000000000 ) ;
#3098 = CARTESIAN_POINT ( 'NONE',  ( 6.013306294175080779, -97.54547149457074795, -4.245374608440741326 ) ) ;
#3099 = ORIENTED_EDGE ( 'NONE', *, *, #8084, .F. ) ;
#3100 = EDGE_CURVE ( 'NONE', #6915, #6387, #4228, .T. ) ;
#3101 = LINE ( 'NONE', #6467, #7463 ) ;
#3102 = STYLED_ITEM ( 'NONE', ( #3979 ), #4379 ) ;
#3103 = ORIENTED_EDGE ( 'NONE', *, *, #2125, .F. ) ;
#3104 = CARTESIAN_POINT ( 'NONE',  ( 45.96623493960122886, -14.74233734943963192, 2.500000000000000888 ) ) ;
#3105 = CARTESIAN_POINT ( 'NONE',  ( -1.529537955723670350, -76.35452850542925773, 5.030887037049979860 ) ) ;
#3106 = CARTESIAN_POINT ( 'NONE',  ( 3.015831842038150690, -91.69547149457073942, -3.989209796945492048 ) ) ;
#3107 = EDGE_CURVE ( 'NONE', #72, #1573, #3767, .T. ) ;
#3108 = CARTESIAN_POINT ( 'NONE',  ( 4.194503406049336469, -65.55452850542924637, -3.171033256558100977 ) ) ;
#3109 = CARTESIAN_POINT ( 'NONE',  ( -1.840261337453200641, -75.19547149457073942, 2.371175808195584267 ) ) ;
#3110 = CARTESIAN_POINT ( 'NONE',  ( -0.09506052544086064648, -81.00452850542926342, -6.999999999999997335 ) ) ;
#3111 = CARTESIAN_POINT ( 'NONE',  ( 4.725907263620374721, -91.09547149457074511, 1.635492904037598283 ) ) ;
#3112 = CARTESIAN_POINT ( 'NONE',  ( 2.862020680886512292, -62.70452850542926626, -4.100960146804039752 ) ) ;
#3113 = CARTESIAN_POINT ( 'NONE',  ( 0.09506052544088100520, -73.50452850542924921, 6.999999999999997335 ) ) ;
#3114 = CARTESIAN_POINT ( 'NONE',  ( -1.069819614139473796, -84.34547149457075932, 2.969112962950044121 ) ) ;
#3115 = ORIENTED_EDGE ( 'NONE', *, *, #6256, .T. ) ;
#3116 = CARTESIAN_POINT ( 'NONE',  ( 45.00000000000000000, -9.999999999999991118, 9.499999999999998224 ) ) ;
#3117 = CARTESIAN_POINT ( 'NONE',  ( 0.09506052544075298261, -58.99547149457073658, -4.999999999999997335 ) ) ;
#3118 = VERTEX_POINT ( 'NONE', #4388 ) ;
#3119 = CARTESIAN_POINT ( 'NONE',  ( -4.725907263620318766, -93.90452850542925489, 1.635492904037698647 ) ) ;
#3120 = CARTESIAN_POINT ( 'NONE',  ( -1.840261337453253487, -63.30452850542926058, -2.371175808195547852 ) ) ;
#3121 = CARTESIAN_POINT ( 'NONE',  ( 0.09506052544087949252, -61.50452850542925631, 6.999999999999997335 ) ) ;
#3122 = CARTESIAN_POINT ( 'NONE',  ( 2.179377348189628361, -69.64547149457072805, 7.030887037049939003 ) ) ;
#3123 = CARTESIAN_POINT ( 'NONE',  ( 0.09506052544075639654, -85.99547149457075079, -4.999999999999997335 ) ) ;
#3124 = CARTESIAN_POINT ( 'NONE',  ( -2.493201789345251829, -79.05452850542926058, 1.934965279058294518 ) ) ;
#3125 = LINE ( 'NONE', #5057, #1610 ) ;
#3126 = EDGE_LOOP ( 'NONE', ( #5435, #6018, #2801, #7528 ) ) ;
#3127 = DIRECTION ( 'NONE',  ( -1.000000000000000000, -8.326672684688674053E-16, 0.000000000000000000 ) ) ;
#3128 = CARTESIAN_POINT ( 'NONE',  ( -2.882544866740875733, -87.60452850542924352, -0.8366430509618996147 ) ) ;
#3129 = CARTESIAN_POINT ( 'NONE',  ( -4.191402346623060104, -66.19547149457073942, 5.607243785695398941 ) ) ;
#3130 = DIRECTION ( 'NONE',  ( 1.000000000000000000, 0.000000000000000000, 0.000000000000000000 ) ) ;
#3131 = PRODUCT ( 'BR-001', 'BR-001', '', ( #3185 ) ) ;
#3132 = CARTESIAN_POINT ( 'NONE',  ( -4.784657899331159925, -62.89547149457074227, 1.454677039711874675 ) ) ;
#3133 = CARTESIAN_POINT ( 'NONE',  ( -4.037591185471542055, -95.29547149457076216, -5.718994135553860936 ) ) ;
#3134 = CARTESIAN_POINT ( 'NONE',  ( 2.882544866740898826, -95.10452850542925773, 0.8366430509618999478 ) ) ;
#3135 = FACE_BOUND ( 'NONE', #4685, .T. ) ;
#3136 = CARTESIAN_POINT ( 'NONE',  ( -2.862020680886494972, -73.20452850542925205, 4.100960146804039752 ) ) ;
#3137 = CARTESIAN_POINT ( 'NONE',  ( 4.194503406049400418, -63.94547149457075363, 3.171033256558012159 ) ) ;
#3138 = ORIENTED_EDGE ( 'NONE', *, *, #6646, .T. ) ;
#3139 = CARTESIAN_POINT ( 'NONE',  ( 50.00000000000000000, -1.734723475976807094E-15, 12.50000000000000000 ) ) ;
#3140 = PRODUCT_RELATED_PRODUCT_CATEGORY ( 'part', '', ( #1716 ) ) ;
#3141 = APPLICATION_PROTOCOL_DEFINITION ( 'draft international standard', 'automotive_design', 1998, #2603 ) ;
#3142 = ORIENTED_EDGE ( 'NONE', *, *, #7212, .F. ) ;
#3143 = VECTOR ( 'NONE', #6320, 1000.000000000000000 ) ;
#3144 = CARTESIAN_POINT ( 'NONE',  ( 54.99999999999999289, 50.00000000000000000, 7.500000000000000000 ) ) ;
#3145 = CARTESIAN_POINT ( 'NONE',  ( -0.09506052544084034328, -75.00452850542924921, -4.999999999999997335 ) ) ;
#3146 = AXIS2_PLACEMENT_3D ( 'NONE', #6708, #7871, #2097 ) ;
#3147 = CARTESIAN_POINT ( 'NONE',  ( -4.312004677470992142, -87.04547149457074795, 3.009306630940933758 ) ) ;
#3148 = ADVANCED_FACE ( 'NONE', ( #5818, #7685 ), #4512, .T. ) ;
#3149 = CARTESIAN_POINT ( 'NONE',  ( 4.387866329943309829, -96.99999999999997158, 0.7004174865519436910 ) ) ;
#3150 = CARTESIAN_POINT ( 'NONE',  ( 1.069819614139493114, -67.84547149457071669, -2.969112962950042789 ) ) ;
#3151 = CARTESIAN_POINT ( 'NONE',  ( 4.191402346623198660, -79.80452850542926058, 5.607243785695311900 ) ) ;
#3152 = CARTESIAN_POINT ( 'NONE',  ( -4.194503406049383543, -86.44547149457071100, -3.171033256558012159 ) ) ;
#3153 = CARTESIAN_POINT ( 'NONE',  ( -5.999999999999992895, -50.00000000000000000, 2.500000000000001776 ) ) ;
#3154 = CARTESIAN_POINT ( 'NONE',  ( 0.09506052544088137990, -76.50452850542926342, 6.999999999999997335 ) ) ;
#3155 = AXIS2_PLACEMENT_3D ( 'NONE', #6255, #2385, #3645 ) ;
#3156 = EDGE_CURVE ( 'NONE', #996, #200, #4347, .T. ) ;
#3157 = CARTESIAN_POINT ( 'NONE',  ( 2.610703060766946138, -85.54547149457074795, -1.773238653441125523 ) ) ;
#3158 = ORIENTED_EDGE ( 'NONE', *, *, #3359, .T. ) ;
#3159 = CARTESIAN_POINT ( 'NONE',  ( 50.00000000000000000, 0.000000000000000000, 0.000000000000000000 ) ) ;
#3160 = LINE ( 'NONE', #3790, #3546 ) ;
#3161 = VECTOR ( 'NONE', #3731, 1000.000000000000114 ) ;
#3162 = ORIENTED_EDGE ( 'NONE', *, *, #520, .F. ) ;
#3163 = CARTESIAN_POINT ( 'NONE',  ( 1.719659006605392504, -88.65452850542926910, 4.969112962950015699 ) ) ;
#3164 = CARTESIAN_POINT ( 'NONE',  ( -1.069819614139541075, -57.15452850542926200, -2.969112962950023249 ) ) ;
#3165 = CARTESIAN_POINT ( 'NONE',  ( 4.194503406049340022, -95.55452850542921794, -3.171033256558100089 ) ) ;
#3166 = CARTESIAN_POINT ( 'NONE',  ( -6.628020296210668683, -65.59547149457073090, -2.253526892787471869 ) ) ;
#3167 = CARTESIAN_POINT ( 'NONE',  ( 4.194503406049403083, -87.94547149457071100, 3.171033256558012159 ) ) ;
#3168 = CARTESIAN_POINT ( 'NONE',  ( -1.069819614139538855, -72.15452850542922647, -2.969112962950023249 ) ) ;
#3169 = CARTESIAN_POINT ( 'NONE',  ( 46.49999999999999289, -14.99999999999999467, 4.499999999999999112 ) ) ;
#3170 = FILL_AREA_STYLE ('',( #6956 ) ) ;
#3171 = CARTESIAN_POINT ( 'NONE',  ( -0.09506052544081743105, -90.00452850542926342, -2.999999999999997780 ) ) ;
#3172 = CARTESIAN_POINT ( 'NONE',  ( -4.191402346623060104, -60.19547149457074653, 5.607243785695398941 ) ) ;
#3173 = CARTESIAN_POINT ( 'NONE',  ( 5.461398254538926800, -97.00000000000000000, -2.077050515704315536 ) ) ;
#3174 = CARTESIAN_POINT ( 'NONE',  ( 2.862020680886597557, -60.79547149457074084, 4.100960146803977580 ) ) ;
#3175 = CARTESIAN_POINT ( 'NONE',  ( 0.09506052544075298261, -58.99547149457073658, -4.999999999999997335 ) ) ;
#3176 = CARTESIAN_POINT ( 'NONE',  ( 3.154386672714811102, -92.25452850542926342, -0.09995255151727241993 ) ) ;
#3177 = DIRECTION ( 'NONE',  ( -0.000000000000000000, 0.000000000000000000, -1.000000000000000000 ) ) ;
#3178 = EDGE_CURVE ( 'NONE', #5499, #4784, #5829, .T. ) ;
#3179 = CARTESIAN_POINT ( 'NONE',  ( 3.015831842038233290, -70.80452850542926058, 3.989209796945429432 ) ) ;
#3180 = CIRCLE ( 'NONE', #347, 1.500000000000001776 ) ;
#3181 = CARTESIAN_POINT ( 'NONE',  ( -4.037591185471542943, -89.29547149457074795, -5.718994135553860936 ) ) ;
#3182 = SHAPE_REPRESENTATION_RELATIONSHIP ( 'NONE' , 'NONE' ,  #6502, #3095 ) ;
#3183 = ORIENTED_EDGE ( 'NONE', *, *, #1946, .T. ) ;
#3184 = DIRECTION ( 'NONE',  ( -1.000000000000000000, 0.000000000000000000, 0.000000000000000000 ) ) ;
#3185 = PRODUCT_CONTEXT ( 'NONE', #3030, 'mechanical' ) ;
#3186 = EDGE_LOOP ( 'NONE', ( #3071, #4990, #1410, #7346 ) ) ;
#3187 = DIRECTION ( 'NONE',  ( 1.000000000000000000, 1.261617073437677752E-16, 0.000000000000000000 ) ) ;
#3188 = CARTESIAN_POINT ( 'NONE',  ( 5.257311121191341918, -77.25452850542926342, -0.09995255151729465215 ) ) ;
#3189 = CARTESIAN_POINT ( 'NONE',  ( -1.719659006605265272, -75.34547149457074511, 4.969112962950051227 ) ) ;
#3190 = CARTESIAN_POINT ( 'NONE',  ( 47.50000000000002132, -54.00000000000000711, 12.50000000000001954 ) ) ;
#3191 = CARTESIAN_POINT ( 'NONE',  ( 1.686450176301635295, -69.79547149457074795, 2.482926158054096000 ) ) ;
#3192 = CARTESIAN_POINT ( 'NONE',  ( 2.369498399071225059, -76.65452850542925489, 6.969112962950009482 ) ) ;
#3193 = CARTESIAN_POINT ( 'NONE',  ( 2.862020680886600221, -84.79547149457074795, 4.100960146803977580 ) ) ;
#3194 = DIRECTION ( 'NONE',  ( 8.326672684688674053E-16, 1.000000000000000000, -0.000000000000000000 ) ) ;
#3195 = CARTESIAN_POINT ( 'NONE',  ( 6.000000000000011546, -100.0010000000000048, 2.500000000000000888 ) ) ;
#3196 = CARTESIAN_POINT ( 'NONE',  ( 6.628020296210642037, -80.40452850542925489, -2.253526892787612645 ) ) ;
#3197 = CARTESIAN_POINT ( 'NONE',  ( -2.610703060766925265, -84.04547149457074795, 1.773238653441125745 ) ) ;
#3198 = ORIENTED_EDGE ( 'NONE', *, *, #2344, .F. ) ;
#3199 = LINE ( 'NONE', #1299, #1744 ) ;
#3200 = DIRECTION ( 'NONE',  ( 1.000000000000000000, 0.000000000000000000, -0.000000000000000000 ) ) ;
#3201 = EDGE_LOOP ( 'NONE', ( #3500, #119, #5362, #3158 ) ) ;
#3202 = CARTESIAN_POINT ( 'NONE',  ( -4.784657899331190123, -78.60452850542925773, -1.454677039711773867 ) ) ;
#3203 = CARTESIAN_POINT ( 'NONE',  ( 0.8796985632579643610, -96.64547149457075648, 3.030887037049952326 ) ) ;
#3204 = AXIS2_PLACEMENT_3D ( 'NONE', #681, #5775, #7814 ) ;
#3205 = CARTESIAN_POINT ( 'NONE',  ( -2.369498399071207739, -60.15452850542926200, -6.969112962950009482 ) ) ;
#3206 = CIRCLE ( 'NONE', #7922, 1.500000000000000666 ) ;
#3207 = CARTESIAN_POINT ( 'NONE',  ( 4.037591185471561595, -72.79547149457074795, 5.718994135553860936 ) ) ;
#3208 = CARTESIAN_POINT ( 'NONE',  ( -1.529537955723776044, -86.14547149457074227, -5.030887037049945221 ) ) ;
#3209 = CARTESIAN_POINT ( 'NONE',  ( 2.823794231030039903, -74.40452850542925489, -1.017458915287783316 ) ) ;
#3210 = CARTESIAN_POINT ( 'NONE',  ( 40.00000000000000000, -14.99999999999999112, 9.499999999999998224 ) ) ;
#3211 = DIRECTION ( 'NONE',  ( -0.000000000000000000, 1.000000000000000000, -0.000000000000000000 ) ) ;
#3212 = CARTESIAN_POINT ( 'NONE',  ( -1.069819614139536412, -90.15452850542926910, -2.969112962950023249 ) ) ;
#3213 = CARTESIAN_POINT ( 'NONE',  ( -6.628020296210668683, -62.59547149457074511, -2.253526892787471869 ) ) ;
#3214 = EDGE_CURVE ( 'NONE', #1841, #4787, #5653, .T. ) ;
#3215 = DIRECTION ( 'NONE',  ( 9.251858538542971581E-17, -1.000000000000000000, 0.000000000000000000 ) ) ;
#3216 = CARTESIAN_POINT ( 'NONE',  ( -4.194503406049383543, -65.44547149457073942, -3.171033256558012159 ) ) ;
#3217 = CARTESIAN_POINT ( 'NONE',  ( -4.725907263620355181, -62.59547149457074511, -1.635492904037597617 ) ) ;
#3218 = CARTESIAN_POINT ( 'NONE',  ( 80.00000000000000000, -2.168404344971008868E-15, 12.50000000000000000 ) ) ;
#3219 = EDGE_CURVE ( 'NONE', #1573, #5004, #6417, .T. ) ;
#3220 = CARTESIAN_POINT ( 'NONE',  ( 47.49999999999999289, -198.2344135219424857, 12.49999999999993960 ) ) ;
#3221 = VECTOR ( 'NONE', #7751, 1000.000000000000000 ) ;
#3222 = CARTESIAN_POINT ( 'NONE',  ( -1.719659006605374074, -63.15452850542925489, -4.969112962950016588 ) ) ;
#3223 = CARTESIAN_POINT ( 'NONE',  ( 6.013306294175080779, -91.54547149457074795, -4.245374608440741326 ) ) ;
#3224 = ORIENTED_EDGE ( 'NONE', *, *, #43, .F. ) ;
#3225 = CARTESIAN_POINT ( 'NONE',  ( 4.312004677471075631, -76.95452850542923784, 3.009306630940844496 ) ) ;
#3226 = DIRECTION ( 'NONE',  ( 1.000000000000000000, 0.000000000000000000, -0.000000000000000000 ) ) ;
#3227 = APPLICATION_PROTOCOL_DEFINITION ( 'draft international standard', 'automotive_design', 1998, #5766 ) ;
#3228 = VECTOR ( 'NONE', #2225, 1000.000000000000114 ) ;
#3229 = DIRECTION ( 'NONE',  ( 1.000000000000000000, 0.000000000000000000, 0.000000000000000000 ) ) ;
#3230 = CARTESIAN_POINT ( 'NONE',  ( -4.194503406049384431, -80.44547149457073942, -3.171033256558012159 ) ) ;
#3231 = CARTESIAN_POINT ( 'NONE',  ( 4.353213783654983793, -96.99999999999998579, 0.1443106696900772756 ) ) ;
#3232 = CARTESIAN_POINT ( 'NONE',  ( 2.823794231030059443, -73.09547149457071669, 1.017458915287723809 ) ) ;
#3233 = CARTESIAN_POINT ( 'NONE',  ( 4.191402346623197772, -73.80452850542926058, 5.607243785695311900 ) ) ;
#3234 = DIRECTION ( 'NONE',  ( -1.000000000000000000, -0.000000000000000000, -0.000000000000000000 ) ) ;
#3235 = CARTESIAN_POINT ( 'NONE',  ( -4.784657899331157260, -80.89547149457074227, 1.454677039711874675 ) ) ;
#3236 = CARTESIAN_POINT ( 'NONE',  ( -1.529537955723671905, -61.35452850542925773, 5.030887037049979860 ) ) ;
#3237 = DIRECTION ( 'NONE',  ( 9.251858538542971828E-16, -1.000000000000000000, 0.000000000000000000 ) ) ;
#3238 = CARTESIAN_POINT ( 'NONE',  ( 0.09506052544088061662, -70.50452850542926342, 6.999999999999997335 ) ) ;
#3239 = CARTESIAN_POINT ( 'NONE',  ( -2.610703060766924821, -87.04547149457074795, 1.773238653441125745 ) ) ;
#3240 = EDGE_CURVE ( 'NONE', #6843, #4159, #1918, .T. ) ;
#3241 = ORIENTED_EDGE ( 'NONE', *, *, #6456, .F. ) ;
#3242 = FACE_OUTER_BOUND ( 'NONE', #3565, .T. ) ;
#3243 = LINE ( 'NONE', #1901, #7996 ) ;
#3244 = CARTESIAN_POINT ( 'NONE',  ( -3.015831842038213750, -90.30452850542926058, -3.989209796945429432 ) ) ;
#3245 = ORIENTED_EDGE ( 'NONE', *, *, #6870, .T. ) ;
#3246 = CARTESIAN_POINT ( 'NONE',  ( 5.257311121191342806, -83.25452850542926342, -0.09995255151729466603 ) ) ;
#3247 = CARTESIAN_POINT ( 'NONE',  ( -3.154386672714792006, -57.75452850542924921, 0.09995255151727280851 ) ) ;
#3248 = CARTESIAN_POINT ( 'NONE',  ( 0.000000000000000000, 0.000000000000000000, 0.000000000000000000 ) ) ;
#3249 = CARTESIAN_POINT ( 'NONE',  ( -4.194503406049315153, -88.05452850542921794, 3.171033256558100533 ) ) ;
#3250 = CARTESIAN_POINT ( 'NONE',  ( -4.037591185471544719, -74.29547149457074795, -5.718994135553860936 ) ) ;
#3251 = CARTESIAN_POINT ( 'NONE',  ( 1.719659006605286145, -79.84547149457073090, -4.969112962950050338 ) ) ;
#3252 = CARTESIAN_POINT ( 'NONE',  ( 1.686450176301584669, -71.70452850542925205, -2.482926158054133303 ) ) ;
#3253 = EDGE_CURVE ( 'NONE', #1902, #6843, #1838, .T. ) ;
#3254 = CARTESIAN_POINT ( 'NONE',  ( 43.45299461620744808, 50.00000000000000000, 7.500000000000000000 ) ) ;
#3255 = DIRECTION ( 'NONE',  ( 0.000000000000000000, -1.000000000000000000, -2.775557561562891844E-16 ) ) ;
#3256 = CARTESIAN_POINT ( 'NONE',  ( -0.8796985632578778747, -88.35452850542924352, 3.030887037049973198 ) ) ;
#3257 = CARTESIAN_POINT ( 'NONE',  ( -4.037591185471546495, -62.29547149457074084, -5.718994135553860936 ) ) ;
#3258 = CARTESIAN_POINT ( 'NONE',  ( 54.99999999999999289, -20.00000000000000000, -7.500000000000000000 ) ) ;
#3259 = CARTESIAN_POINT ( 'NONE',  ( -4.312004677471057867, -72.45452850542922363, -3.009306630940844052 ) ) ;
#3260 = CARTESIAN_POINT ( 'NONE',  ( -6.013306294175056799, -96.04547149457074795, 4.245374608440741326 ) ) ;
#3261 = CARTESIAN_POINT ( 'NONE',  ( 75.00000000000000000, -20.00000000000000355, 7.499999999999993783 ) ) ;
#3262 = DIRECTION ( 'NONE',  ( -1.000000000000000000, 0.000000000000000000, 0.000000000000000000 ) ) ;
#3263 = CARTESIAN_POINT ( 'NONE',  ( 4.784657899331207886, -62.10452850542925063, 1.454677039711774533 ) ) ;
#3264 = CARTESIAN_POINT ( 'NONE',  ( 6.686770931921479644, -91.39547149457074227, -2.072711028461788896 ) ) ;
#3265 = SURFACE_SIDE_STYLE ('',( #7648 ) ) ;
#3266 = ORIENTED_EDGE ( 'NONE', *, *, #6508, .T. ) ;
#3267 = CARTESIAN_POINT ( 'NONE',  ( 2.862020680886513624, -71.70452850542925205, -4.100960146804039752 ) ) ;
#3268 = CARTESIAN_POINT ( 'NONE',  ( 43.50000000000000711, -14.99999999999999467, 9.499999999999996447 ) ) ;
#3269 = EDGE_CURVE ( 'NONE', #2962, #5374, #6925, .T. ) ;
#3270 = VECTOR ( 'NONE', #6665, 1000.000000000000000 ) ;
#3271 = ADVANCED_FACE ( 'NONE', ( #3726, #3135 ), #1158, .T. ) ;
#3272 = LINE ( 'NONE', #1370, #7722 ) ;
#3273 = CARTESIAN_POINT ( 'NONE',  ( -2.862020680886580681, -77.29547149457074795, -4.100960146803977580 ) ) ;
#3274 = CARTESIAN_POINT ( 'NONE',  ( 4.226755616500139645, -97.00000000000000000, 2.333567455633055676 ) ) ;
#3275 = CARTESIAN_POINT ( 'NONE',  ( 2.823794231030058111, -64.09547149457071669, 1.017458915287723809 ) ) ;
#3276 = CARTESIAN_POINT ( 'NONE',  ( -4.037591185471423927, -67.20452850542925205, 5.718994135553947977 ) ) ;
#3277 = FACE_OUTER_BOUND ( 'NONE', #1770, .T. ) ;
#3278 = CARTESIAN_POINT ( 'NONE',  ( -4.784657899331158148, -77.89547149457074227, 1.454677039711874675 ) ) ;
#3279 = CARTESIAN_POINT ( 'NONE',  ( -4.784657899331192787, -57.60452850542925773, -1.454677039711773867 ) ) ;
#3280 = CARTESIAN_POINT ( 'NONE',  ( 3.015831842038234623, -82.80452850542926058, 3.989209796945429432 ) ) ;
#3281 = CARTESIAN_POINT ( 'NONE',  ( -4.037591185471424815, -64.20452850542925205, 5.718994135553947977 ) ) ;
#3282 = CARTESIAN_POINT ( 'NONE',  ( -1.686450176301616644, -80.29547149457074795, -2.482926158054096000 ) ) ;
#3283 = ADVANCED_FACE ( 'NONE', ( #1877 ), #6339, .T. ) ;
#3284 = VECTOR ( 'NONE', #4315, 1000.000000000000000 ) ;
#3285 = EDGE_LOOP ( 'NONE', ( #580, #956, #8162, #2790, #4169, #3956, #6303, #6820 ) ) ;
#3286 = DIRECTION ( 'NONE',  ( 1.000000000000000000, -8.326672684688674053E-16, 0.000000000000000000 ) ) ;
#3287 = CARTESIAN_POINT ( 'NONE',  ( 4.312004677471078296, -91.95452850542925205, 3.009306630940844496 ) ) ;
#3288 = CARTESIAN_POINT ( 'NONE',  ( 4.784657899331211439, -92.10452850542925773, 1.454677039711774533 ) ) ;
#3289 = ORIENTED_EDGE ( 'NONE', *, *, #280, .T. ) ;
#3290 = CARTESIAN_POINT ( 'NONE',  ( -5.257311121191323267, -81.75452850542926342, 0.09995255151729529053 ) ) ;
#3291 = CARTESIAN_POINT ( 'NONE',  ( -3.154386672714787565, -95.74547149457073658, -0.09995255151720625064 ) ) ;
#3292 = DIRECTION ( 'NONE',  ( 1.000000000000000000, 0.000000000000000000, 0.000000000000000000 ) ) ;
#3293 = CARTESIAN_POINT ( 'NONE',  ( -2.862020680886493196, -85.20452850542925205, 4.100960146804039752 ) ) ;
#3294 = VECTOR ( 'NONE', #48, 1000.000000000000000 ) ;
#3295 = AXIS2_PLACEMENT_3D ( 'NONE', #2016, #693, #6600 ) ;
#3296 = COLOUR_RGB ( '', 0.66274510, 0.83137255, 0.94901961) ;
#3297 = CARTESIAN_POINT ( 'NONE',  ( -7.360235569667860744, -62.74547149457073658, -0.09995255151716124498 ) ) ;
#3298 = CARTESIAN_POINT ( 'NONE',  ( -1.069819614139539521, -66.15452850542925489, -2.969112962950023249 ) ) ;
#3299 = CARTESIAN_POINT ( 'NONE',  ( 50.00000000000000000, -12.00000000000000355, -12.50000000000000178 ) ) ;
#3300 = CARTESIAN_POINT ( 'NONE',  ( 1.500000000000001998, -26.99999999999998934, -7.000000000000000000 ) ) ;
#3301 = CARTESIAN_POINT ( 'NONE',  ( -2.882544866740875733, -90.60452850542925773, -0.8366430509618996147 ) ) ;
#3302 = CARTESIAN_POINT ( 'NONE',  ( -0.09506052544085875911, -96.00452850542926342, -6.999999999999997335 ) ) ;
#3303 = DIRECTION ( 'NONE',  ( 1.000000000000000000, 0.000000000000000000, 0.000000000000000000 ) ) ;
#3304 = CARTESIAN_POINT ( 'NONE',  ( -1.719659006605371632, -81.15452850542922647, -4.969112962950016588 ) ) ;
#3305 = CARTESIAN_POINT ( 'NONE',  ( 4.191402346623080533, -91.69547149457075363, -5.607243785695398941 ) ) ;
#3306 = DIRECTION ( 'NONE',  ( -2.775557561562892337E-16, 1.000000000000000000, -0.000000000000000000 ) ) ;
#3307 = CARTESIAN_POINT ( 'NONE',  ( 55.00000000000002132, -88.00000000000000000, 0.000000000000000000 ) ) ;
#3308 = CARTESIAN_POINT ( 'NONE',  ( -1.719659006605374518, -60.15452850542926200, -4.969112962950016588 ) ) ;
#3309 = APPLICATION_CONTEXT ( 'automotive_design' ) ;
#3310 = CARTESIAN_POINT ( 'NONE',  ( -4.037591185471543831, -86.29547149457074795, -5.718994135553860936 ) ) ;
#3311 = ORIENTED_EDGE ( 'NONE', *, *, #3214, .T. ) ;
#3312 = CARTESIAN_POINT ( 'NONE',  ( 3.015831842038233734, -76.80452850542926058, 3.989209796945429432 ) ) ;
#3313 = CARTESIAN_POINT ( 'NONE',  ( -47.50000000000000711, -49.99999999999998579, 12.49999999999993960 ) ) ;
#3314 = ITEM_DEFINED_TRANSFORMATION ( 'NONE', 'NONE', #2549,  #2840 ) ;
#3315 = LINE ( 'NONE', #5830, #2608 ) ;
#3316 = CARTESIAN_POINT ( 'NONE',  ( 1.719659006605286367, -82.84547149457074511, -4.969112962950050338 ) ) ;
#3317 = DIRECTION ( 'NONE',  ( 0.000000000000000000, -0.7071067811865466846, -0.7071067811865484609 ) ) ;
#3318 = CARTESIAN_POINT ( 'NONE',  ( 0.09506052544077478461, -64.99547149457075079, -2.999999999999997780 ) ) ;
#3319 = CARTESIAN_POINT ( 'NONE',  ( -2.369498399071207739, -66.15452850542925489, -6.969112962950009482 ) ) ;
#3320 = LINE ( 'NONE', #2102, #6828 ) ;
#3321 = CARTESIAN_POINT ( 'NONE',  ( -2.862020680886579793, -83.29547149457074795, -4.100960146803977580 ) ) ;
#3322 = CARTESIAN_POINT ( 'NONE',  ( 4.312004677471073855, -58.95452850542925205, 3.009306630940844496 ) ) ;
#3323 = CARTESIAN_POINT ( 'NONE',  ( 2.862020680886515400, -86.70452850542925205, -4.100960146804039752 ) ) ;
#3324 = CARTESIAN_POINT ( 'NONE',  ( 4.037591185471441690, -71.70452850542925205, -5.718994135553947977 ) ) ;
#3325 = EDGE_CURVE ( 'NONE', #4798, #6658, #557, .T. ) ;
#3326 = CARTESIAN_POINT ( 'NONE',  ( 2.610703060766946138, -82.54547149457074795, -1.773238653441125523 ) ) ;
#3327 = VERTEX_POINT ( 'NONE', #3848 ) ;
#3328 = DIRECTION ( 'NONE',  ( -1.000000000000000000, -0.000000000000000000, 0.000000000000000000 ) ) ;
#3329 = DIRECTION ( 'NONE',  ( -0.000000000000000000, -0.000000000000000000, -1.000000000000000000 ) ) ;
#3330 = CARTESIAN_POINT ( 'NONE',  ( -1.719659006605371188, -84.15452850542925489, -4.969112962950016588 ) ) ;
#3331 = ORIENTED_EDGE ( 'NONE', *, *, #7782, .F. ) ;
#3332 = CARTESIAN_POINT ( 'NONE',  ( 1.719659006605392060, -85.65452850542924068, 4.969112962950015699 ) ) ;
#3333 = CARTESIAN_POINT ( 'NONE',  ( -1.069819614139472463, -90.34547149457073090, 2.969112962950044121 ) ) ;
#3334 = DIRECTION ( 'NONE',  ( 1.228736747721611495E-48, 0.000000000000000000, -1.000000000000000000 ) ) ;
#3335 = CARTESIAN_POINT ( 'NONE',  ( 0.09506052544086121547, -85.50452850542926342, 4.999999999999997335 ) ) ;
#3336 = CARTESIAN_POINT ( 'NONE',  ( -2.179377348189613262, -59.14547149457074227, -7.030887037049939003 ) ) ;
#3337 = CARTESIAN_POINT ( 'NONE',  ( 0.8796985632578971925, -62.85452850542923642, -3.030887037049972310 ) ) ;
#3338 = DIRECTION ( 'NONE',  ( 0.000000000000000000, 1.000000000000000000, 0.000000000000000000 ) ) ;
#3339 = PRESENTATION_LAYER_ASSIGNMENT (  '', '', ( #4809 ) ) ;
#3340 = LINE ( 'NONE', #675, #7950 ) ;
#3341 = CARTESIAN_POINT ( 'NONE',  ( 2.610703060766983885, -73.95452850542925205, 1.773238653441072232 ) ) ;
#3342 = CARTESIAN_POINT ( 'NONE',  ( -6.013306294175150946, -84.45452850542925205, -4.245374608440613429 ) ) ;
#3343 = FACE_OUTER_BOUND ( 'NONE', #2899, .T. ) ;
#3344 = CARTESIAN_POINT ( 'NONE',  ( 6.628020296210689111, -85.09547149457075932, 2.253526892787472757 ) ) ;
#3345 = PLANE ( 'NONE',  #3204 ) ;
#3346 = DIRECTION ( 'NONE',  ( -0.000000000000000000, -1.387778780781445676E-16, 1.000000000000000000 ) ) ;
#3347 = CARTESIAN_POINT ( 'NONE',  ( 3.154386672714808437, -70.24547149457075079, 0.09995255151720662534 ) ) ;
#3348 = EDGE_CURVE ( 'NONE', #4787, #524, #1792, .T. ) ;
#3349 = ORIENTED_EDGE ( 'NONE', *, *, #4025, .T. ) ;
#3350 = CARTESIAN_POINT ( 'NONE',  ( 4.194503406049337357, -74.55452850542923215, -3.171033256558100089 ) ) ;
#3351 = CARTESIAN_POINT ( 'NONE',  ( 4.191402346623081421, -94.69547149457076785, -5.607243785695398941 ) ) ;
#3352 = VERTEX_POINT ( 'NONE', #8274 ) ;
#3353 = CARTESIAN_POINT ( 'NONE',  ( -5.257311121191324155, -78.75452850542924921, 0.09995255151729526277 ) ) ;
#3354 = FACE_OUTER_BOUND ( 'NONE', #1179, .T. ) ;
#3355 = AXIS2_PLACEMENT_3D ( 'NONE', #1480, #1562, #7252 ) ;
#3356 = EDGE_CURVE ( 'NONE', #2974, #348, #5143, .T. ) ;
#3357 = FACE_OUTER_BOUND ( 'NONE', #2405, .T. ) ;
#3358 =( GEOMETRIC_REPRESENTATION_CONTEXT ( 3 ) GLOBAL_UNCERTAINTY_ASSIGNED_CONTEXT ( ( #5447 ) ) GLOBAL_UNIT_ASSIGNED_CONTEXT ( ( #2380, #388, #3594 ) ) REPRESENTATION_CONTEXT ( 'NONE', 'WORKASPACE' ) );
#3359 = EDGE_CURVE ( 'NONE', #4798, #5382, #636, .T. ) ;
#3360 = CARTESIAN_POINT ( 'NONE',  ( -1.529537955723777154, -77.14547149457074227, -5.030887037049945221 ) ) ;
#3361 = DIRECTION ( 'NONE',  ( 0.000000000000000000, 8.673617379884033007E-17, 1.000000000000000000 ) ) ;
#3362 = CARTESIAN_POINT ( 'NONE',  ( 3.154386672714807105, -64.24547149457075079, 0.09995255151720662534 ) ) ;
#3363 = AXIS2_PLACEMENT_3D ( 'NONE', #5603, #7472, #7591 ) ;
#3364 = CARTESIAN_POINT ( 'NONE',  ( -6.013306294175152722, -69.45452850542925205, -4.245374608440613429 ) ) ;
#3365 = CARTESIAN_POINT ( 'NONE',  ( 6.123233995736760366E-16, -26.99999999999998934, -7.000000000000000000 ) ) ;
#3366 = CARTESIAN_POINT ( 'NONE',  ( -4.784657899331158148, -74.89547149457074227, 1.454677039711874675 ) ) ;
#3367 = CARTESIAN_POINT ( 'NONE',  ( 3.943604702053941724E-15, -27.99999999999999645, 2.500000000000000888 ) ) ;
#3368 = CARTESIAN_POINT ( 'NONE',  ( 4.784657899331211439, -89.10452850542925773, 1.454677039711774533 ) ) ;
#3369 = CARTESIAN_POINT ( 'NONE',  ( -4.037591185471423927, -67.20452850542925205, 5.718994135553947977 ) ) ;
#3370 = AXIS2_PLACEMENT_3D ( 'NONE', #1605, #4170, #971 ) ;
#3371 = CARTESIAN_POINT ( 'NONE',  ( -2.882544866740857969, -77.89547149457074227, 0.8366430509619596778 ) ) ;
#3372 = ORIENTED_EDGE ( 'NONE', *, *, #5640, .F. ) ;
#3373 = DIRECTION ( 'NONE',  ( 0.000000000000000000, -1.000000000000000000, -2.168404344971010101E-16 ) ) ;
#3374 = DIRECTION ( 'NONE',  ( 1.000000000000000000, 0.000000000000000000, -0.000000000000000000 ) ) ;
#3375 = CARTESIAN_POINT ( 'NONE',  ( 5.257311121191342806, -86.25452850542924921, -0.09995255151729465215 ) ) ;
#3376 = ORIENTED_EDGE ( 'NONE', *, *, #1880, .T. ) ;
#3377 = CARTESIAN_POINT ( 'NONE',  ( 0.09506052544086121547, -85.50452850542926342, 4.999999999999997335 ) ) ;
#3378 = CARTESIAN_POINT ( 'NONE',  ( -0.09506052544075481447, -90.49547149457075079, 2.999999999999997780 ) ) ;
#3379 = EDGE_CURVE ( 'NONE', #8124, #5238, #8118, .T. ) ;
#3380 =( GEOMETRIC_REPRESENTATION_CONTEXT ( 3 ) GLOBAL_UNCERTAINTY_ASSIGNED_CONTEXT ( ( #7302 ) ) GLOBAL_UNIT_ASSIGNED_CONTEXT ( ( #2972, #4989, #7775 ) ) REPRESENTATION_CONTEXT ( 'NONE', 'WORKASPACE' ) );
#3381 = CARTESIAN_POINT ( 'NONE',  ( 0.000000000000000000, 0.000000000000000000, 0.000000000000000000 ) ) ;
#3382 = CARTESIAN_POINT ( 'NONE',  ( -4.784657899331189235, -90.60452850542925773, -1.454677039711773867 ) ) ;
#3383 = CARTESIAN_POINT ( 'NONE',  ( 5.895805022753492608, -60.94547149457074653, 4.407101234057782868 ) ) ;
#3384 = CARTESIAN_POINT ( 'NONE',  ( -2.882544866740878398, -69.60452850542924352, -0.8366430509618996147 ) ) ;
#3385 =( GEOMETRIC_REPRESENTATION_CONTEXT ( 3 ) GLOBAL_UNCERTAINTY_ASSIGNED_CONTEXT ( ( #6117 ) ) GLOBAL_UNIT_ASSIGNED_CONTEXT ( ( #1409, #7864, #6671 ) ) REPRESENTATION_CONTEXT ( 'NONE', 'WORKASPACE' ) );
#3386 = CARTESIAN_POINT ( 'NONE',  ( 40.00000000000000000, -14.99999999999999289, 4.500000000000000888 ) ) ;
#3387 = DIRECTION ( 'NONE',  ( -9.251858538542971581E-17, 1.000000000000000000, -0.000000000000000000 ) ) ;
#3388 = CARTESIAN_POINT ( 'NONE',  ( -2.823794231030021251, -75.90452850542925489, 1.017458915287783316 ) ) ;
#3389 = CARTESIAN_POINT ( 'NONE',  ( -6.013306294175149169, -87.45452850542925205, -4.245374608440613429 ) ) ;
#3390 = LINE ( 'NONE', #174, #2114 ) ;
#3391 = CARTESIAN_POINT ( 'NONE',  ( -0.09506052544071229293, -90.49547149457075079, 6.999999999999997335 ) ) ;
#3392 = DIRECTION ( 'NONE',  ( 0.000000000000000000, 0.000000000000000000, -1.000000000000000000 ) ) ;
#3393 = FACE_OUTER_BOUND ( 'NONE', #7666, .T. ) ;
#3394 = CARTESIAN_POINT ( 'NONE',  ( 1.840261337453219292, -67.69547149457073942, -2.371175808195584267 ) ) ;
#3395 = CARTESIAN_POINT ( 'NONE',  ( -2.862020680886496748, -58.20452850542925916, 4.100960146804039752 ) ) ;
#3396 = ORIENTED_EDGE ( 'NONE', *, *, #7440, .T. ) ;
#3397 = CARTESIAN_POINT ( 'NONE',  ( 4.194503406049335581, -68.55452850542926058, -3.171033256558100089 ) ) ;
#3398 = CARTESIAN_POINT ( 'NONE',  ( 2.179377348189630137, -84.64547149457074227, 7.030887037049939003 ) ) ;
#3399 = ORIENTED_EDGE ( 'NONE', *, *, #3356, .F. ) ;
#3400 = CARTESIAN_POINT ( 'NONE',  ( -4.194503406049316041, -79.05452850542921794, 3.171033256558100533 ) ) ;
#3401 = CARTESIAN_POINT ( 'NONE',  ( 47.50000000000000000, -49.99999999999999289, -12.50000000000000888 ) ) ;
#3402 = CARTESIAN_POINT ( 'NONE',  ( -5.257311121191324155, -65.74547149457073658, -0.09995255151718371311 ) ) ;
#3403 = DIRECTION ( 'NONE',  ( -0.000000000000000000, -0.000000000000000000, -1.000000000000000000 ) ) ;
#3404 = CARTESIAN_POINT ( 'NONE',  ( -2.610703060766927930, -60.04547149457073374, 1.773238653441125745 ) ) ;
#3405 = CARTESIAN_POINT ( 'NONE',  ( -6.686770931921506289, -66.60452850542924352, -2.072711028461647675 ) ) ;
#3406 = PLANE ( 'NONE',  #5741 ) ;
#3407 = EDGE_CURVE ( 'NONE', #97, #2766, #1318, .T. ) ;
#3408 = CARTESIAN_POINT ( 'NONE',  ( -1.719659006605370744, -87.15452850542926910, -4.969112962950016588 ) ) ;
#3409 = CARTESIAN_POINT ( 'NONE',  ( 4.191402346623195996, -64.80452850542926058, 5.607243785695311900 ) ) ;
#3410 = CARTESIAN_POINT ( 'NONE',  ( -2.610703060766925709, -81.04547149457074795, 1.773238653441125745 ) ) ;
#3411 = ADVANCED_FACE ( 'NONE', ( #8314 ), #5276, .F. ) ;
#3412 = VERTEX_POINT ( 'NONE', #3468 ) ;
#3413 = FACE_OUTER_BOUND ( 'NONE', #4437, .T. ) ;
#3414 = CYLINDRICAL_SURFACE ( 'NONE', #5691, 1.500000000000001776 ) ;
#3415 = CARTESIAN_POINT ( 'NONE',  ( 1.529537955723692111, -89.85452850542925773, -5.030887037049978971 ) ) ;
#3416 = VERTEX_POINT ( 'NONE', #5319 ) ;
#3417 = CARTESIAN_POINT ( 'NONE',  ( -4.725907263620321430, -75.90452850542925489, 1.635492904037698647 ) ) ;
#3418 = CARTESIAN_POINT ( 'NONE',  ( -1.686450176301614645, -95.29547149457076216, -2.482926158054096000 ) ) ;
#3419 = CARTESIAN_POINT ( 'NONE',  ( -4.784657899331190123, -84.60452850542927195, -1.454677039711773867 ) ) ;
#3420 = CARTESIAN_POINT ( 'NONE',  ( 6.686770931921476979, -64.39547149457074227, -2.072711028461788896 ) ) ;
#3421 = VECTOR ( 'NONE', #6765, 1000.000000000000000 ) ;
#3422 = CARTESIAN_POINT ( 'NONE',  ( 2.493201789345270480, -65.55452850542926058, -1.934965279058294518 ) ) ;
#3423 = CARTESIAN_POINT ( 'NONE',  ( 63.45299461620744808, 100.0000000000000000, -7.500000000000000000 ) ) ;
#3424 = FACE_OUTER_BOUND ( 'NONE', #3186, .T. ) ;
#3425 = CARTESIAN_POINT ( 'NONE',  ( 2.493201789345271369, -77.55452850542926058, -1.934965279058294518 ) ) ;
#3426 = AXIS2_PLACEMENT_3D ( 'NONE', #382, #3510, #8027 ) ;
#3427 = CARTESIAN_POINT ( 'NONE',  ( 6.013306294175171374, -85.95452850542925205, 4.245374608440616093 ) ) ;
#3428 = CIRCLE ( 'NONE', #2222, 5.000000000000004441 ) ;
#3429 = CARTESIAN_POINT ( 'NONE',  ( 7.360235569667878508, -85.24547149457075079, 0.09995255151716216091 ) ) ;
#3430 = CARTESIAN_POINT ( 'NONE',  ( -65.00000000000000000, 0.000000000000000000, 0.000000000000000000 ) ) ;
#3431 = CARTESIAN_POINT ( 'NONE',  ( -65.00000000000000000, -12.00000000000000355, -12.50000000000000178 ) ) ;
#3432 = CARTESIAN_POINT ( 'NONE',  ( -1.069819614139475350, -72.34547149457073090, 2.969112962950044121 ) ) ;
#3433 = UNCERTAINTY_MEASURE_WITH_UNIT (LENGTH_MEASURE( 1.000000000000000082E-05 ), #1797, 'distance_accuracy_value', 'NONE');
#3434 = CARTESIAN_POINT ( 'NONE',  ( 50.00000000000000000, -9.999999999999994671, 0.000000000000000000 ) ) ;
#3435 = ORIENTED_EDGE ( 'NONE', *, *, #3835, .F. ) ;
#3436 = CARTESIAN_POINT ( 'NONE',  ( 3.015831842038232846, -67.80452850542926058, 3.989209796945429432 ) ) ;
#3437 = CARTESIAN_POINT ( 'NONE',  ( -7.360235569667858968, -77.74547149457073658, -0.09995255151716124498 ) ) ;
#3438 = ORIENTED_EDGE ( 'NONE', *, *, #4555, .T. ) ;
#3439 = CARTESIAN_POINT ( 'NONE',  ( 2.862020680886512736, -65.70452850542925205, -4.100960146804039752 ) ) ;
#3440 = EDGE_CURVE ( 'NONE', #6387, #6901, #4720, .T. ) ;
#3441 = DIRECTION ( 'NONE',  ( -1.000000000000000000, 0.000000000000000000, 0.000000000000000000 ) ) ;
#3442 = CARTESIAN_POINT ( 'NONE',  ( -1.529537955723777820, -68.14547149457075648, -5.030887037049945221 ) ) ;
#3443 = LINE ( 'NONE', #7356, #5777 ) ;
#3444 = CARTESIAN_POINT ( 'NONE',  ( 2.882544866740875289, -61.39547149457074937, -0.8366430509619593447 ) ) ;
#3445 = CARTESIAN_POINT ( 'NONE',  ( -7.360235569667860744, -60.75452850542924921, 0.09995255151731782806 ) ) ;
#3446 = EDGE_LOOP ( 'NONE', ( #5213, #6347, #7281, #2570 ) ) ;
#3447 = CARTESIAN_POINT ( 'NONE',  ( 1.719659006605392504, -88.65452850542925489, 4.969112962950016588 ) ) ;
#3448 = CARTESIAN_POINT ( 'NONE',  ( -0.09506052544086292244, -63.00452850542925631, -6.999999999999997335 ) ) ;
#3449 = CARTESIAN_POINT ( 'NONE',  ( -0.8796985632579421566, -83.14547149457072805, -3.030887037049952326 ) ) ;
#3450 = ORIENTED_EDGE ( 'NONE', *, *, #2206, .F. ) ;
#3451 = FACE_OUTER_BOUND ( 'NONE', #6987, .T. ) ;
#3452 = DIRECTION ( 'NONE',  ( 1.000000000000000000, 0.000000000000000000, 0.000000000000000000 ) ) ;
#3453 = CARTESIAN_POINT ( 'NONE',  ( -4.194503406049316041, -82.05452850542924637, 3.171033256558100533 ) ) ;
#3454 = ORIENTED_EDGE ( 'NONE', *, *, #3661, .T. ) ;
#3455 = CARTESIAN_POINT ( 'NONE',  ( -2.862020680886494528, -76.20452850542926626, 4.100960146804039752 ) ) ;
#3456 = CARTESIAN_POINT ( 'NONE',  ( -2.493201789345290020, -86.44547149457073942, -1.934965279058240561 ) ) ;
#3457 = CARTESIAN_POINT ( 'NONE',  ( -4.725907263620350740, -95.59547149457074511, -1.635492904037597617 ) ) ;
#3458 = CARTESIAN_POINT ( 'NONE',  ( 4.725907263620340082, -74.40452850542925489, -1.635492904037697981 ) ) ;
#3459 = CARTESIAN_POINT ( 'NONE',  ( 2.179377348189484032, -92.85452850542924352, -7.030887037049986077 ) ) ;
#3460 = CARTESIAN_POINT ( 'NONE',  ( -2.610703060766966122, -69.45452850542925205, -1.773238653441072232 ) ) ;
#3461 = ORIENTED_EDGE ( 'NONE', *, *, #4629, .F. ) ;
#3462 = CARTESIAN_POINT ( 'NONE',  ( 75.00000000000000000, -20.00000000000000000, 7.500000000000000000 ) ) ;
#3463 = LINE ( 'NONE', #5520, #5915 ) ;
#3464 = CARTESIAN_POINT ( 'NONE',  ( -0.09506052544081895761, -78.00452850542926342, -2.999999999999997780 ) ) ;
#3465 = CARTESIAN_POINT ( 'NONE',  ( 6.013306294175171374, -91.95452850542925205, 4.245374608440616093 ) ) ;
#3466 = CARTESIAN_POINT ( 'NONE',  ( -6.013306294175058575, -90.04547149457074795, 4.245374608440741326 ) ) ;
#3467 = PLANE ( 'NONE',  #7371 ) ;
#3468 = CARTESIAN_POINT ( 'NONE',  ( -47.50000000000000711, -20.00000000000000355, 12.49999999999999112 ) ) ;
#3469 = CARTESIAN_POINT ( 'NONE',  ( -0.8796985632579442660, -65.14547149457074227, -3.030887037049952326 ) ) ;
#3470 = PRESENTATION_STYLE_ASSIGNMENT (( #897 ) ) ;
#3471 = ORIENTED_EDGE ( 'NONE', *, *, #1545, .F. ) ;
#3472 = EDGE_CURVE ( 'NONE', #6782, #3690, #6891, .T. ) ;
#3473 = CARTESIAN_POINT ( 'NONE',  ( -5.257311121191324155, -69.75452850542926342, 0.09995255151729526277 ) ) ;
#3474 = CARTESIAN_POINT ( 'NONE',  ( 7.360235569667878508, -85.24547149457075079, 0.09995255151716216091 ) ) ;
#3475 = ORIENTED_EDGE ( 'NONE', *, *, #1880, .F. ) ;
#3476 = CARTESIAN_POINT ( 'NONE',  ( -4.784657899331191011, -66.60452850542924352, -1.454677039711773867 ) ) ;
#3477 = CARTESIAN_POINT ( 'NONE',  ( 47.49999999999999289, -19.99999999999999645, -12.50000000000000000 ) ) ;
#3478 = CARTESIAN_POINT ( 'NONE',  ( -4.784657899331159037, -71.89547149457074227, 1.454677039711874675 ) ) ;
#3479 = CARTESIAN_POINT ( 'NONE',  ( 0.7550207793516368060, -97.00000000000001421, -3.949353336951454629 ) ) ;
#3480 = CARTESIAN_POINT ( 'NONE',  ( -4.194503406049381766, -95.44547149457071100, -3.171033256558012159 ) ) ;
#3481 = CARTESIAN_POINT ( 'NONE',  ( 2.179377348189480035, -62.85452850542923642, -7.030887037049986077 ) ) ;
#3482 = ORIENTED_EDGE ( 'NONE', *, *, #5442, .F. ) ;
#3483 = LINE ( 'NONE', #7197, #5034 ) ;
#3484 = CARTESIAN_POINT ( 'NONE',  ( 4.784657899331210551, -80.10452850542925773, 1.454677039711774533 ) ) ;
#3485 = ORIENTED_EDGE ( 'NONE', *, *, #5515, .F. ) ;
#3486 = CIRCLE ( 'NONE', #6845, 1.500000000000000666 ) ;
#3487 = DIRECTION ( 'NONE',  ( 0.000000000000000000, -1.000000000000000000, 0.000000000000000000 ) ) ;
#3488 = CARTESIAN_POINT ( 'NONE',  ( -1.529537955723668352, -91.35452850542921510, 5.030887037049979860 ) ) ;
#3489 = CARTESIAN_POINT ( 'NONE',  ( -4.784657899331190123, -75.60452850542925773, -1.454677039711773867 ) ) ;
#3490 = ORIENTED_EDGE ( 'NONE', *, *, #2626, .F. ) ;
#3491 = CARTESIAN_POINT ( 'NONE',  ( 2.862020680886514068, -74.70452850542926626, -4.100960146804039752 ) ) ;
#3492 = CARTESIAN_POINT ( 'NONE',  ( 0.09506052544077857325, -94.99547149457075079, -2.999999999999997780 ) ) ;
#3493 = CARTESIAN_POINT ( 'NONE',  ( 2.610703060766943029, -61.54547149457074084, -1.773238653441125523 ) ) ;
#3494 = CARTESIAN_POINT ( 'NONE',  ( -5.257311121191324155, -78.75452850542924921, 0.09995255151729526277 ) ) ;
#3495 = CARTESIAN_POINT ( 'NONE',  ( -6.686770931921503625, -87.60452850542924352, -2.072711028461647675 ) ) ;
#3496 = CARTESIAN_POINT ( 'NONE',  ( 1.686450176301638626, -96.79547149457073374, 2.482926158054096000 ) ) ;
#3497 = VERTEX_POINT ( 'NONE', #2759 ) ;
#3498 = CARTESIAN_POINT ( 'NONE',  ( -1.500000000000000666, -26.99999999999998934, -7.000000000000000000 ) ) ;
#3499 = AXIS2_PLACEMENT_3D ( 'NONE', #7376, #335, #2952 ) ;
#3500 = ORIENTED_EDGE ( 'NONE', *, *, #6196, .T. ) ;
#3501 = CARTESIAN_POINT ( 'NONE',  ( 75.00000000000000000, -9.999999999999994671, 1.500000000000000666 ) ) ;
#3502 = CARTESIAN_POINT ( 'NONE',  ( -1.840261337453251267, -81.30452850542926058, -2.371175808195547852 ) ) ;
#3503 = CARTESIAN_POINT ( 'NONE',  ( 5.895805022753407343, -86.55452850542926058, -4.407101234057908989 ) ) ;
#3504 = CARTESIAN_POINT ( 'NONE',  ( 4.037591185471563371, -81.79547149457074795, 5.718994135553860936 ) ) ;
#3505 = DIRECTION ( 'NONE',  ( 1.000000000000000000, 0.000000000000000000, 0.000000000000000000 ) ) ;
#3506 = PRODUCT_DEFINITION ( 'UNKNOWN', '', #7807, #6790 ) ;
#3507 = CARTESIAN_POINT ( 'NONE',  ( 3.750550224659021659, -96.89549487877602019, 3.480863915964662159 ) ) ;
#3508 = CARTESIAN_POINT ( 'NONE',  ( 3.154386672714807549, -67.24547149457075079, 0.09995255151720662534 ) ) ;
#3509 = PRODUCT_DEFINITION_CONTEXT ( 'detailed design', #3309, 'design' ) ;
#3510 = DIRECTION ( 'NONE',  ( 1.000000000000000000, 9.251858538542972814E-17, -0.000000000000000000 ) ) ;
#3511 = ORIENTED_EDGE ( 'NONE', *, *, #5697, .T. ) ;
#3512 = CARTESIAN_POINT ( 'NONE',  ( 80.00000000000000000, -20.00000000000000355, 12.49999999999999645 ) ) ;
#3513 = CARTESIAN_POINT ( 'NONE',  ( 2.862020680886512736, -65.70452850542925205, -4.100960146804039752 ) ) ;
#3514 = CARTESIAN_POINT ( 'NONE',  ( -4.037591185471544719, -77.29547149457074795, -5.718994135553860936 ) ) ;
#3515 = EDGE_LOOP ( 'NONE', ( #4016, #3980 ) ) ;
#3516 = CARTESIAN_POINT ( 'NONE',  ( -5.257311121191325043, -77.74547149457072237, -0.09995255151718372699 ) ) ;
#3517 = CARTESIAN_POINT ( 'NONE',  ( 5.257311121191341918, -64.24547149457073658, 0.09995255151718437925 ) ) ;
#3518 = CARTESIAN_POINT ( 'NONE',  ( -4.194503406049320482, -64.05452850542926058, 3.171033256558100533 ) ) ;
#3519 = CARTESIAN_POINT ( 'NONE',  ( 40.00000000000000000, -19.99999999999999645, 4.500000000000000000 ) ) ;
#3520 = CARTESIAN_POINT ( 'NONE',  ( -2.862020680886581125, -71.29547149457074795, -4.100960146803977580 ) ) ;
#3521 = DIRECTION ( 'NONE',  ( 1.000000000000000000, 0.000000000000000000, 0.000000000000000000 ) ) ;
#3522 = CARTESIAN_POINT ( 'NONE',  ( 6.013306294175167821, -58.95452850542925916, 4.245374608440616093 ) ) ;
#3523 = ORIENTED_EDGE ( 'NONE', *, *, #583, .F. ) ;
#3524 = ADVANCED_FACE ( 'NONE', ( #723 ), #1363, .T. ) ;
#3525 = ORIENTED_EDGE ( 'NONE', *, *, #2729, .F. ) ;
#3526 = CARTESIAN_POINT ( 'NONE',  ( 50.00000000000000000, -12.00000000000000711, 12.49999999999999822 ) ) ;
#3527 = CARTESIAN_POINT ( 'NONE',  ( -4.725907263620320542, -84.90452850542925489, 1.635492904037698647 ) ) ;
#3528 = CARTESIAN_POINT ( 'NONE',  ( 4.194503406049337357, -77.55452850542926058, -3.171033256558100089 ) ) ;
#3529 = ORIENTED_EDGE ( 'NONE', *, *, #5266, .T. ) ;
#3530 = CARTESIAN_POINT ( 'NONE',  ( 3.015831842038233290, -70.80452850542926058, 3.989209796945429432 ) ) ;
#3531 = CARTESIAN_POINT ( 'NONE',  ( 2.610703060766946138, -82.54547149457074795, -1.773238653441125523 ) ) ;
#3532 = CARTESIAN_POINT ( 'NONE',  ( 0.8796985632579598091, -60.64547149457074227, 3.030887037049952326 ) ) ;
#3533 = CARTESIAN_POINT ( 'NONE',  ( 4.312004677471075631, -73.95452850542926626, 3.009306630940844496 ) ) ;
#3534 = CARTESIAN_POINT ( 'NONE',  ( 6.686770931921525829, -92.10452850542925773, 2.072711028461649008 ) ) ;
#3535 = EDGE_CURVE ( 'NONE', #5499, #7328, #1445, .T. ) ;
#3536 = CARTESIAN_POINT ( 'NONE',  ( -1.840261337453254153, -57.30452850542924637, -2.371175808195547852 ) ) ;
#3537 = ORIENTED_EDGE ( 'NONE', *, *, #3070, .F. ) ;
#3538 = CARTESIAN_POINT ( 'NONE',  ( -80.00000000000000000, -20.00000000000000355, 12.49999999999999645 ) ) ;
#3539 = ORIENTED_EDGE ( 'NONE', *, *, #1582, .F. ) ;
#3540 = CARTESIAN_POINT ( 'NONE',  ( -2.823794231030022583, -63.90452850542925489, 1.017458915287783316 ) ) ;
#3541 = CARTESIAN_POINT ( 'NONE',  ( 6.628020296210642037, -80.40452850542925489, -2.253526892787612645 ) ) ;
#3542 = CARTESIAN_POINT ( 'NONE',  ( 2.369498399071078509, -82.84547149457074511, -6.969112962950057444 ) ) ;
#3543 = CARTESIAN_POINT ( 'NONE',  ( 45.00000000000000000, -15.00000000000000178, 4.500000000000000000 ) ) ;
#3544 = CARTESIAN_POINT ( 'NONE',  ( 1.529537955723797582, -93.64547149457074227, 5.030887037049945221 ) ) ;
#3545 = CARTESIAN_POINT ( 'NONE',  ( -3.154386672714788453, -84.75452850542926342, 0.09995255151727280851 ) ) ;
#3546 = VECTOR ( 'NONE', #6361, 1000.000000000000000 ) ;
#3547 = AXIS2_PLACEMENT_3D ( 'NONE', #3526, #5301, #3373 ) ;
#3548 = ORIENTED_EDGE ( 'NONE', *, *, #3269, .T. ) ;
#3549 = FACE_BOUND ( 'NONE', #4600, .T. ) ;
#3550 = CARTESIAN_POINT ( 'NONE',  ( 5.257311121191341918, -65.25452850542926342, -0.09995255151729465215 ) ) ;
#3551 = CARTESIAN_POINT ( 'NONE',  ( 6.628020296210689111, -85.09547149457075932, 2.253526892787472757 ) ) ;
#3552 = PRESENTATION_STYLE_ASSIGNMENT (( #7350 ) ) ;
#3553 = EDGE_LOOP ( 'NONE', ( #961, #8296, #2133, #4075, #4703, #7206, #401, #1260 ) ) ;
#3554 = CARTESIAN_POINT ( 'NONE',  ( -4.312004677470993030, -75.04547149457074795, 3.009306630940933314 ) ) ;
#3555 = CARTESIAN_POINT ( 'NONE',  ( -1.529537955723777820, -71.14547149457071384, -5.030887037049945221 ) ) ;
#3556 = AXIS2_PLACEMENT_3D ( 'NONE', #7519, #1581, #6461 ) ;
#3557 = CARTESIAN_POINT ( 'NONE',  ( 4.312004677471073855, -61.95452850542923784, 3.009306630940844496 ) ) ;
#3558 = DIRECTION ( 'NONE',  ( 1.000000000000000000, 0.000000000000000000, 0.000000000000000000 ) ) ;
#3559 = AXIS2_PLACEMENT_3D ( 'NONE', #4949, #1038, #4874 ) ;
#3560 = CARTESIAN_POINT ( 'NONE',  ( 4.312004677471011682, -73.54547149457073374, -3.009306630940933314 ) ) ;
#3561 = FILL_AREA_STYLE_COLOUR ( '', #8083 ) ;
#3562 = CARTESIAN_POINT ( 'NONE',  ( 1.529537955723692999, -95.85452850542922931, -5.030887037049978971 ) ) ;
#3563 = ORIENTED_EDGE ( 'NONE', *, *, #7749, .F. ) ;
#3564 = CARTESIAN_POINT ( 'NONE',  ( 54.99999999999999289, -9.999999999999994671, -1.500000000000000666 ) ) ;
#3565 = EDGE_LOOP ( 'NONE', ( #5016, #360, #3777, #7028, #242, #1519, #1467, #7503 ) ) ;
#3566 = FACE_OUTER_BOUND ( 'NONE', #3446, .T. ) ;
#3567 = CARTESIAN_POINT ( 'NONE',  ( -4.784657899331189235, -87.60452850542925773, -1.454677039711773867 ) ) ;
#3568 = CARTESIAN_POINT ( 'NONE',  ( 2.862020680886514068, -74.70452850542926626, -4.100960146804039752 ) ) ;
#3569 = ORIENTED_EDGE ( 'NONE', *, *, #974, .F. ) ;
#3570 = CARTESIAN_POINT ( 'NONE',  ( 4.194503406049338246, -74.55452850542924637, -3.171033256558100977 ) ) ;
#3571 = CARTESIAN_POINT ( 'NONE',  ( 1.840261337453220625, -76.69547149457073942, -2.371175808195584267 ) ) ;
#3572 =( REPRESENTATION_RELATIONSHIP ('NONE','NONE', #4188, #6502 ) REPRESENTATION_RELATIONSHIP_WITH_TRANSFORMATION ( #4024 )SHAPE_REPRESENTATION_RELATIONSHIP( ) );
#3573 = CARTESIAN_POINT ( 'NONE',  ( 3.015831842038151578, -97.69547149457075363, -3.989209796945492048 ) ) ;
#3574 = EDGE_CURVE ( 'NONE', #4272, #8085, #2047, .T. ) ;
#3575 = CARTESIAN_POINT ( 'NONE',  ( 1.719659006605389173, -64.65452850542925489, 4.969112962950016588 ) ) ;
#3576 = CARTESIAN_POINT ( 'NONE',  ( 7.360235569667880284, -86.25452850542924921, -0.09995255151731691212 ) ) ;
#3577 = CARTESIAN_POINT ( 'NONE',  ( 0.8796985632578967484, -59.85452850542925773, -3.030887037049972310 ) ) ;
#3578 = APPLICATION_PROTOCOL_DEFINITION ( 'draft international standard', 'automotive_design', 1998, #6318 ) ;
#3579 = ORIENTED_EDGE ( 'NONE', *, *, #3325, .T. ) ;
#3580 = DIRECTION ( 'NONE',  ( 0.000000000000000000, 0.000000000000000000, 1.000000000000000000 ) ) ;
#3581 = ORIENTED_EDGE ( 'NONE', *, *, #7144, .T. ) ;
#3582 = ADVANCED_BREP_SHAPE_REPRESENTATION ( '', ( #7136, #2840 ), #3385 ) ;
#3583 = CARTESIAN_POINT ( 'NONE',  ( -0.09506052544083767875, -96.00452850542926342, -4.999999999999997335 ) ) ;
#3584 = CARTESIAN_POINT ( 'NONE',  ( -1.686450176301566906, -67.20452850542925205, 2.482926158054133303 ) ) ;
#3585 = CARTESIAN_POINT ( 'NONE',  ( 7.360235569667878508, -82.24547149457073658, 0.09995255151716216091 ) ) ;
#3586 = CARTESIAN_POINT ( 'NONE',  ( 45.00000000000000000, -9.999999999999991118, 9.499999999999998224 ) ) ;
#3587 = CARTESIAN_POINT ( 'NONE',  ( 80.00000000000000000, -20.00000000000000355, 12.49999999999999645 ) ) ;
#3588 = CARTESIAN_POINT ( 'NONE',  ( -0.09506052544081780575, -87.00452850542926342, -2.999999999999997780 ) ) ;
#3589 =( NAMED_UNIT ( * ) SI_UNIT ( $, .STERADIAN. ) SOLID_ANGLE_UNIT ( ) );
#3590 = ORIENTED_EDGE ( 'NONE', *, *, #5011, .T. ) ;
#3591 = DIRECTION ( 'NONE',  ( 0.000000000000000000, 0.000000000000000000, 1.000000000000000000 ) ) ;
#3592 = CARTESIAN_POINT ( 'NONE',  ( 1.686450176301588000, -95.70452850542928047, -2.482926158054133303 ) ) ;
#3593 = CARTESIAN_POINT ( 'NONE',  ( -6.013306294175061240, -72.04547149457074795, 4.245374608440741326 ) ) ;
#3594 =( NAMED_UNIT ( * ) SI_UNIT ( $, .STERADIAN. ) SOLID_ANGLE_UNIT ( ) );
#3595 = LINE ( 'NONE', #266, #6119 ) ;
#3596 = PRODUCT_DEFINITION_SHAPE ( 'NONE', 'NONE',  #3506 ) ;
#3597 = CARTESIAN_POINT ( 'NONE',  ( -5.257311121191325043, -74.74547149457073658, -0.09995255151718372699 ) ) ;
#3598 = CARTESIAN_POINT ( 'NONE',  ( 4.784657899331176800, -70.39547149457074227, -1.454677039711874009 ) ) ;
#3599 = CARTESIAN_POINT ( 'NONE',  ( 4.784657899331207886, -62.10452850542925063, 1.454677039711774533 ) ) ;
#3600 = DIRECTION ( 'NONE',  ( 0.000000000000000000, 0.000000000000000000, 1.000000000000000000 ) ) ;
#3601 = EDGE_CURVE ( 'NONE', #204, #1012, #2799, .T. ) ;
#3602 = CARTESIAN_POINT ( 'NONE',  ( -0.09506052544073692601, -63.49547149457074369, 4.999999999999997335 ) ) ;
#3603 = VECTOR ( 'NONE', #2124, 1000.000000000000000 ) ;
#3604 =( NAMED_UNIT ( * ) PLANE_ANGLE_UNIT ( ) SI_UNIT ( $, .RADIAN. ) );
#3605 = CARTESIAN_POINT ( 'NONE',  ( 4.784657899331212327, -95.10452850542925773, 1.454677039711774533 ) ) ;
#3606 = ORIENTED_EDGE ( 'NONE', *, *, #167, .T. ) ;
#3607 = UNCERTAINTY_MEASURE_WITH_UNIT (LENGTH_MEASURE( 1.000000000000000082E-05 ), #7000, 'distance_accuracy_value', 'NONE');
#3608 = DIRECTION ( 'NONE',  ( 1.000000000000000000, -0.000000000000000000, -0.000000000000000000 ) ) ;
#3609 = ADVANCED_FACE ( 'NONE', ( #7857 ), #765, .F. ) ;
#3610 = EDGE_LOOP ( 'NONE', ( #7750, #5914, #1899, #939 ) ) ;
#3611 = CARTESIAN_POINT ( 'NONE',  ( 3.943604702053941724E-15, -27.99999999999999645, -2.499999999999999112 ) ) ;
#3612 = CARTESIAN_POINT ( 'NONE',  ( -4.312004677471056091, -90.45452850542926626, -3.009306630940844052 ) ) ;
#3613 = CARTESIAN_POINT ( 'NONE',  ( 5.257311121191341918, -80.25452850542922079, -0.09995255151729465215 ) ) ;
#3614 = CARTESIAN_POINT ( 'NONE',  ( -1.719659006605374074, -63.15452850542925489, -4.969112962950015699 ) ) ;
#3615 = CARTESIAN_POINT ( 'NONE',  ( 3.154386672714809325, -76.24547149457073658, 0.09995255151720662534 ) ) ;
#3616 = CARTESIAN_POINT ( 'NONE',  ( -0.8796985632579448211, -62.14547149457074937, -3.030887037049952326 ) ) ;
#3617 = CARTESIAN_POINT ( 'NONE',  ( 4.725907263620340082, -71.40452850542925489, -1.635492904037697981 ) ) ;
#3618 = CARTESIAN_POINT ( 'NONE',  ( 2.179377348189482699, -83.85452850542927195, -7.030887037049986077 ) ) ;
#3619 = CARTESIAN_POINT ( 'NONE',  ( 1.686450176301583337, -59.70452850542925916, -2.482926158054133303 ) ) ;
#3620 = VECTOR ( 'NONE', #4636, 1000.000000000000114 ) ;
#3621 = DIRECTION ( 'NONE',  ( 0.000000000000000000, 0.000000000000000000, 1.000000000000000000 ) ) ;
#3622 = VERTEX_POINT ( 'NONE', #6583 ) ;
#3623 = FACE_OUTER_BOUND ( 'NONE', #4276, .T. ) ;
#3624 = ADVANCED_FACE ( 'NONE', ( #3393 ), #5951, .T. ) ;
#3625 = CARTESIAN_POINT ( 'NONE',  ( -1.719659006605370744, -93.15452850542925489, -4.969112962950015699 ) ) ;
#3626 = CARTESIAN_POINT ( 'NONE',  ( 1.069819614139556396, -70.65452850542925489, 2.969112962950023249 ) ) ;
#3627 = STYLED_ITEM ( 'NONE', ( #1831 ), #1677 ) ;
#3628 = CARTESIAN_POINT ( 'NONE',  ( 6.686770931921477867, -79.39547149457074227, -2.072711028461788896 ) ) ;
#3629 = CARTESIAN_POINT ( 'NONE',  ( 0.09506052544086235345, -94.50452850542926342, 4.999999999999997335 ) ) ;
#3630 = CARTESIAN_POINT ( 'NONE',  ( 5.257311121191343695, -94.24547149457072237, 0.09995255151718437925 ) ) ;
#3631 = CARTESIAN_POINT ( 'NONE',  ( 1.686450176301586890, -89.70452850542925205, -2.482926158054133303 ) ) ;
#3632 = PRODUCT_DEFINITION_SHAPE ( 'NONE', 'NONE',  #8350 ) ;
#3633 = EDGE_CURVE ( 'NONE', #2855, #4621, #177, .T. ) ;
#3634 = AXIS2_PLACEMENT_3D ( 'NONE', #823, #3403, #7404 ) ;
#3635 = CARTESIAN_POINT ( 'NONE',  ( 50.00000000000000000, 1.734723475976807094E-15, -12.50000000000000000 ) ) ;
#3636 = ORIENTED_EDGE ( 'NONE', *, *, #2399, .F. ) ;
#3637 = CARTESIAN_POINT ( 'NONE',  ( 50.00000000000000000, -9.999999999999994671, 0.000000000000000000 ) ) ;
#3638 = CARTESIAN_POINT ( 'NONE',  ( 1.686450176301587334, -92.70452850542926626, -2.482926158054133303 ) ) ;
#3639 = CARTESIAN_POINT ( 'NONE',  ( -4.191402346623058328, -72.19547149457073942, 5.607243785695398941 ) ) ;
#3640 = CARTESIAN_POINT ( 'NONE',  ( 5.604172532792750516, -97.00000000000004263, 0.4687073228881366016 ) ) ;
#3641 = COLOUR_RGB ( '', 0.66274510, 0.83137255, 0.94901961) ;
#3642 = CARTESIAN_POINT ( 'NONE',  ( -4.194503406049383543, -74.44547149457072521, -3.171033256558012159 ) ) ;
#3643 = CARTESIAN_POINT ( 'NONE',  ( -2.862020680886582014, -65.29547149457073374, -4.100960146803977580 ) ) ;
#3644 = CARTESIAN_POINT ( 'NONE',  ( -4.784657899331192787, -57.60452850542925773, -1.454677039711773867 ) ) ;
#3645 = DIRECTION ( 'NONE',  ( 1.000000000000000000, 0.000000000000000000, 0.000000000000000000 ) ) ;
#3646 = CARTESIAN_POINT ( 'NONE',  ( -4.784657899331160813, -59.89547149457074227, 1.454677039711874675 ) ) ;
#3647 = CARTESIAN_POINT ( 'NONE',  ( -2.862020680886492308, -94.20452850542926626, 4.100960146804039752 ) ) ;
#3648 = ORIENTED_EDGE ( 'NONE', *, *, #2171, .F. ) ;
#3649 = PLANE ( 'NONE',  #5699 ) ;
#3650 = VERTEX_POINT ( 'NONE', #2676 ) ;
#3651 = CARTESIAN_POINT ( 'NONE',  ( -47.50000000000000711, -198.2344135219424857, 12.49999999999993960 ) ) ;
#3652 = CARTESIAN_POINT ( 'NONE',  ( 0.09506052544086121547, -85.50452850542926342, 4.999999999999997335 ) ) ;
#3653 = CARTESIAN_POINT ( 'NONE',  ( 1.529537955723796472, -87.64547149457071384, 5.030887037049945221 ) ) ;
#3654 = ADVANCED_FACE ( 'NONE', ( #3932 ), #3974, .F. ) ;
#3655 = CARTESIAN_POINT ( 'NONE',  ( -3.015831842038216859, -63.30452850542925347, -3.989209796945429432 ) ) ;
#3656 = CARTESIAN_POINT ( 'NONE',  ( -1.840261337453199975, -81.19547149457073942, 2.371175808195584267 ) ) ;
#3657 = CARTESIAN_POINT ( 'NONE',  ( -3.015831842038127597, -87.19547149457073942, 3.989209796945492048 ) ) ;
#3658 = CARTESIAN_POINT ( 'NONE',  ( 4.194503406049335581, -65.55452850542923215, -3.171033256558100089 ) ) ;
#3659 = CARTESIAN_POINT ( 'NONE',  ( -6.628020296210620721, -75.90452850542925489, 2.253526892787613978 ) ) ;
#3660 = CARTESIAN_POINT ( 'NONE',  ( 2.823794231030062107, -94.09547149457074511, 1.017458915287723809 ) ) ;
#3661 = EDGE_CURVE ( 'NONE', #5740, #1450, #5994, .T. ) ;
#3662 = VERTEX_POINT ( 'NONE', #850 ) ;
#3663 = CARTESIAN_POINT ( 'NONE',  ( 63.45299461620744808, 100.0000000000000000, 7.500000000000000000 ) ) ;
#3664 = PRODUCT ( 'arm', 'arm', '', ( #5516 ) ) ;
#3665 = CARTESIAN_POINT ( 'NONE',  ( -2.862020680886492308, -94.20452850542926626, 4.100960146804039752 ) ) ;
#3666 = CARTESIAN_POINT ( 'NONE',  ( -2.823794231030021695, -72.90452850542925489, 1.017458915287783316 ) ) ;
#3667 = CARTESIAN_POINT ( 'NONE',  ( 1.529537955723692555, -92.85452850542925773, -5.030887037049978971 ) ) ;
#3668 = CARTESIAN_POINT ( 'NONE',  ( -6.628020296210667794, -74.59547149457071669, -2.253526892787471869 ) ) ;
#3669 = CARTESIAN_POINT ( 'NONE',  ( 1.529537955723692555, -92.85452850542925773, -5.030887037049978971 ) ) ;
#3670 = VECTOR ( 'NONE', #3346, 1000.000000000000000 ) ;
#3671 = CARTESIAN_POINT ( 'NONE',  ( 1.719659006605287477, -91.84547149457074511, -4.969112962950050338 ) ) ;
#3672 = CARTESIAN_POINT ( 'NONE',  ( 0.8796985632578997460, -83.85452850542927195, -3.030887037049972310 ) ) ;
#3673 = DIRECTION ( 'NONE',  ( -0.000000000000000000, 1.000000000000000000, 2.168404344971010347E-16 ) ) ;
#3674 = ORIENTED_EDGE ( 'NONE', *, *, #7070, .F. ) ;
#3675 = LINE ( 'NONE', #2455, #3015 ) ;
#3676 = CARTESIAN_POINT ( 'NONE',  ( 1.529537955723688336, -59.85452850542924352, -5.030887037049978971 ) ) ;
#3677 = CARTESIAN_POINT ( 'NONE',  ( 0.09506052544073349819, -70.99547149457075079, -6.999999999999997335 ) ) ;
#3678 = DIRECTION ( 'NONE',  ( 0.000000000000000000, 0.000000000000000000, 1.000000000000000000 ) ) ;
#3679 = CARTESIAN_POINT ( 'NONE',  ( -5.108479284279210399E-14, -97.00000000000000000, -5.999999999999992006 ) ) ;
#3680 = CARTESIAN_POINT ( 'NONE',  ( 2.862020680886598001, -63.79547149457074084, 4.100960146803977580 ) ) ;
#3681 = CARTESIAN_POINT ( 'NONE',  ( 1.529537955723794695, -66.64547149457071384, 5.030887037049945221 ) ) ;
#3682 = CARTESIAN_POINT ( 'NONE',  ( -2.493201789345250052, -91.05452850542926058, 1.934965279058294518 ) ) ;
#3683 = CARTESIAN_POINT ( 'NONE',  ( 47.50000000000002132, -51.00000000000000711, -12.50000000000001954 ) ) ;
#3684 = VECTOR ( 'NONE', #2067, 1000.000000000000000 ) ;
#3685 = CIRCLE ( 'NONE', #4615, 1.500000000000000666 ) ;
#3686 = CARTESIAN_POINT ( 'NONE',  ( -4.194503406049316929, -73.05452850542926058, 3.171033256558100533 ) ) ;
#3687 = CARTESIAN_POINT ( 'NONE',  ( -1.529537955723778930, -59.14547149457072805, -5.030887037049945221 ) ) ;
#3688 = VECTOR ( 'NONE', #5113, 1000.000000000000000 ) ;
#3689 = COLOUR_RGB ( '', 0.31764706, 0.68627451, 0.89019608) ;
#3690 = VERTEX_POINT ( 'NONE', #2084 ) ;
#3691 = FACE_BOUND ( 'NONE', #8047, .T. ) ;
#3692 = EDGE_CURVE ( 'NONE', #3690, #6782, #435, .T. ) ;
#3693 =( GEOMETRIC_REPRESENTATION_CONTEXT ( 3 ) GLOBAL_UNCERTAINTY_ASSIGNED_CONTEXT ( ( #1077 ) ) GLOBAL_UNIT_ASSIGNED_CONTEXT ( ( #5419, #4610, #1588 ) ) REPRESENTATION_CONTEXT ( 'NONE', 'WORKASPACE' ) );
#3694 = ORIENTED_EDGE ( 'NONE', *, *, #931, .T. ) ;
#3695 = DIRECTION ( 'NONE',  ( -1.000000000000000000, 0.000000000000000000, 0.000000000000000000 ) ) ;
#3696 = CARTESIAN_POINT ( 'NONE',  ( 5.257311121191341918, -80.25452850542922079, -0.09995255151729465215 ) ) ;
#3697 = CARTESIAN_POINT ( 'NONE',  ( 2.862020680886601109, -90.79547149457074795, 4.100960146803977580 ) ) ;
#3698 = CARTESIAN_POINT ( 'NONE',  ( -1.529537955723672571, -58.35452850542925063, 5.030887037049979860 ) ) ;
#3699 = CARTESIAN_POINT ( 'NONE',  ( 2.823794231030060775, -85.09547149457075932, 1.017458915287723809 ) ) ;
#3700 = CARTESIAN_POINT ( 'NONE',  ( 6.013306294175169597, -76.95452850542926626, 4.245374608440616093 ) ) ;
#3701 = CARTESIAN_POINT ( 'NONE',  ( 4.312004677471013459, -85.54547149457070532, -3.009306630940933314 ) ) ;
#3702 = CARTESIAN_POINT ( 'NONE',  ( -5.257311121191324155, -63.75452850542925631, 0.09995255151729526277 ) ) ;
#3703 = CARTESIAN_POINT ( 'NONE',  ( -2.369498399071206407, -78.15452850542924068, -6.969112962950009482 ) ) ;
#3704 = CARTESIAN_POINT ( 'NONE',  ( 0.09506052544077779609, -88.99547149457075079, -2.999999999999997780 ) ) ;
#3705 = VERTEX_POINT ( 'NONE', #4097 ) ;
#3706 = CARTESIAN_POINT ( 'NONE',  ( -5.999999999999993783, -47.00000000000000000, 2.500000000000000888 ) ) ;
#3707 = CARTESIAN_POINT ( 'NONE',  ( -5.999999999999995559, -27.99999999999999645, -2.499999999999999112 ) ) ;
#3708 = ORIENTED_EDGE ( 'NONE', *, *, #5412, .T. ) ;
#3709 = CARTESIAN_POINT ( 'NONE',  ( 4.725907263620341858, -89.40452850542926910, -1.635492904037697981 ) ) ;
#3710 = CARTESIAN_POINT ( 'NONE',  ( -3.154386672714791118, -66.75452850542926342, 0.09995255151727280851 ) ) ;
#3711 = CARTESIAN_POINT ( 'NONE',  ( -2.179377348189463603, -58.35452850542927195, 7.030887037049988741 ) ) ;
#3712 = CARTESIAN_POINT ( 'NONE',  ( -7.360235569667858968, -71.74547149457075079, -0.09995255151716124498 ) ) ;
#3713 = CARTESIAN_POINT ( 'NONE',  ( 6.000000000000012434, -50.00000000000000000, -2.499999999999999112 ) ) ;
#3714 = CARTESIAN_POINT ( 'NONE',  ( 4.784657899331178577, -85.39547149457074227, -1.454677039711874009 ) ) ;
#3715 = CARTESIAN_POINT ( 'NONE',  ( 3.154386672714809325, -77.25452850542924921, -0.09995255151727241993 ) ) ;
#3716 = DIRECTION ( 'NONE',  ( 0.000000000000000000, -0.000000000000000000, 1.000000000000000000 ) ) ;
#3717 = EDGE_CURVE ( 'NONE', #8255, #184, #894, .T. ) ;
#3718 = ORIENTED_EDGE ( 'NONE', *, *, #5762, .F. ) ;
#3719 = DIRECTION ( 'NONE',  ( 1.000000000000000000, 0.000000000000000000, -0.000000000000000000 ) ) ;
#3720 = CARTESIAN_POINT ( 'NONE',  ( 2.610703060766986106, -94.95452850542926626, 1.773238653441072232 ) ) ;
#3721 = CARTESIAN_POINT ( 'NONE',  ( -4.191402346623058328, -75.19547149457073942, 5.607243785695398941 ) ) ;
#3722 = CARTESIAN_POINT ( 'NONE',  ( 4.302742873392585210, -96.99999999999947420, 2.548615363087012753 ) ) ;
#3723 = CARTESIAN_POINT ( 'NONE',  ( -2.862020680886582014, -62.29547149457074084, -4.100960146803977580 ) ) ;
#3724 = CARTESIAN_POINT ( 'NONE',  ( -0.09506052544071151578, -96.49547149457075079, 6.999999999999997335 ) ) ;
#3725 = CARTESIAN_POINT ( 'NONE',  ( 1.719659006605388285, -58.65452850542924068, 4.969112962950016588 ) ) ;
#3726 = FACE_OUTER_BOUND ( 'NONE', #442, .T. ) ;
#3727 = ADVANCED_FACE ( 'NONE', ( #6034 ), #4639, .F. ) ;
#3728 = CARTESIAN_POINT ( 'NONE',  ( 0.09506052544085895339, -67.50452850542926342, 4.999999999999997335 ) ) ;
#3729 = CARTESIAN_POINT ( 'NONE',  ( -2.369498399071054529, -96.34547149457074511, 6.969112962950058332 ) ) ;
#3730 = VERTEX_POINT ( 'NONE', #3587 ) ;
#3731 = DIRECTION ( 'NONE',  ( 0.9662349396012461789, 0.2576626505603324402, 0.000000000000000000 ) ) ;
#3732 = AXIS2_PLACEMENT_3D ( 'NONE', #1778, #421, #7507 ) ;
#3733 = VERTEX_POINT ( 'NONE', #1654 ) ;
#3734 = FACE_BOUND ( 'NONE', #2312, .T. ) ;
#3735 = CARTESIAN_POINT ( 'NONE',  ( 4.194503406049338246, -80.55452850542926058, -3.171033256558100089 ) ) ;
#3736 = CARTESIAN_POINT ( 'NONE',  ( 4.312004677471013459, -85.54547149457070532, -3.009306630940933314 ) ) ;
#3737 = CARTESIAN_POINT ( 'NONE',  ( 3.015831842038232402, -64.80452850542926058, 3.989209796945429432 ) ) ;
#3738 = CARTESIAN_POINT ( 'NONE',  ( 1.069819614139493558, -70.84547149457073090, -2.969112962950042789 ) ) ;
#3739 = CARTESIAN_POINT ( 'NONE',  ( 0.09506052544088137990, -76.50452850542926342, 6.999999999999997335 ) ) ;
#3740 = CARTESIAN_POINT ( 'NONE',  ( -3.015831842038127153, -90.19547149457073942, 3.989209796945492048 ) ) ;
#3741 = CARTESIAN_POINT ( 'NONE',  ( -0.09506052544084186984, -63.00452850542925631, -4.999999999999997335 ) ) ;
#3742 = CARTESIAN_POINT ( 'NONE',  ( -6.686770931921506289, -78.60452850542927195, -2.072711028461647675 ) ) ;
#3743 = CARTESIAN_POINT ( 'NONE',  ( -2.610703060766923933, -90.04547149457074795, 1.773238653441125745 ) ) ;
#3744 = VERTEX_POINT ( 'NONE', #6155 ) ;
#3745 = DIRECTION ( 'NONE',  ( -0.000000000000000000, -0.000000000000000000, -1.000000000000000000 ) ) ;
#3746 = PLANE ( 'NONE',  #5432 ) ;
#3747 = EDGE_LOOP ( 'NONE', ( #2949, #8139, #324, #5581 ) ) ;
#3748 = CARTESIAN_POINT ( 'NONE',  ( 2.862020680886515844, -89.70452850542926626, -4.100960146804039752 ) ) ;
#3749 = CARTESIAN_POINT ( 'NONE',  ( 2.882544866740894829, -62.10452850542925063, 0.8366430509618999478 ) ) ;
#3750 = CARTESIAN_POINT ( 'NONE',  ( 0.09506052544087911782, -58.50452850542925631, 6.999999999999997335 ) ) ;
#3751 = VECTOR ( 'NONE', #7106, 1000.000000000000000 ) ;
#3752 = CARTESIAN_POINT ( 'NONE',  ( 7.360235569667877620, -73.24547149457075079, 0.09995255151716216091 ) ) ;
#3753 = VECTOR ( 'NONE', #2832, 1000.000000000000000 ) ;
#3754 = CARTESIAN_POINT ( 'NONE',  ( 2.862020680886599777, -81.79547149457073374, 4.100960146803977580 ) ) ;
#3755 = CARTESIAN_POINT ( 'NONE',  ( 0.8796985632578988579, -74.85452850542925773, -3.030887037049972310 ) ) ;
#3756 = VECTOR ( 'NONE', #6457, 1000.000000000000000 ) ;
#3757 = CARTESIAN_POINT ( 'NONE',  ( 50.00000000000000000, -9.999999999999994671, -1.500000000000000666 ) ) ;
#3758 = ORIENTED_EDGE ( 'NONE', *, *, #4641, .F. ) ;
#3759 = CARTESIAN_POINT ( 'NONE',  ( -47.50000000000000711, -198.2344135219424857, -12.50000000000005151 ) ) ;
#3760 = CARTESIAN_POINT ( 'NONE',  ( -2.862020680886496748, -58.20452850542925916, 4.100960146804039752 ) ) ;
#3761 = VECTOR ( 'NONE', #2577, 1000.000000000000000 ) ;
#3762 = CARTESIAN_POINT ( 'NONE',  ( 4.191402346623077868, -67.69547149457073942, -5.607243785695398941 ) ) ;
#3763 = LINE ( 'NONE', #5569, #4827 ) ;
#3764 = CARTESIAN_POINT ( 'NONE',  ( 4.312004677471010794, -67.54547149457074795, -3.009306630940932425 ) ) ;
#3765 = CARTESIAN_POINT ( 'NONE',  ( -5.257311121191324155, -62.74547149457075079, -0.09995255151718371311 ) ) ;
#3766 = CARTESIAN_POINT ( 'NONE',  ( 0.8796985632579013004, -95.85452850542924352, -3.030887037049972310 ) ) ;
#3767 = LINE ( 'NONE', #6964, #8264 ) ;
#3768 = EDGE_CURVE ( 'NONE', #2188, #480, #7428, .T. ) ;
#3769 = CARTESIAN_POINT ( 'NONE',  ( -5.257311121191324155, -72.75452850542924921, 0.09995255151729526277 ) ) ;
#3770 = CARTESIAN_POINT ( 'NONE',  ( -6.628020296210665130, -95.59547149457074511, -2.253526892787471869 ) ) ;
#3771 =( NAMED_UNIT ( * ) SI_UNIT ( $, .STERADIAN. ) SOLID_ANGLE_UNIT ( ) );
#3772 = EDGE_LOOP ( 'NONE', ( #832, #2183, #6164, #6972 ) ) ;
#3773 = EDGE_CURVE ( 'NONE', #5980, #2822, #2877, .T. ) ;
#3774 = LINE ( 'NONE', #5033, #6781 ) ;
#3775 = MECHANICAL_DESIGN_GEOMETRIC_PRESENTATION_REPRESENTATION (  '', ( #3102 ), #672 ) ;
#3776 = APPLICATION_PROTOCOL_DEFINITION ( 'draft international standard', 'automotive_design', 1998, #883 ) ;
#3777 = ORIENTED_EDGE ( 'NONE', *, *, #2171, .T. ) ;
#3778 = DIRECTION ( 'NONE',  ( 0.000000000000000000, 0.000000000000000000, 1.000000000000000000 ) ) ;
#3779 = CARTESIAN_POINT ( 'NONE',  ( 0.09506052544086046607, -79.50452850542926342, 4.999999999999997335 ) ) ;
#3780 = CARTESIAN_POINT ( 'NONE',  ( 4.312004677471013459, -91.54547149457074795, -3.009306630940933314 ) ) ;
#3781 = CARTESIAN_POINT ( 'NONE',  ( -4.784657899331192787, -57.60452850542925773, -1.454677039711773867 ) ) ;
#3782 = CARTESIAN_POINT ( 'NONE',  ( -1.840261337453200863, -72.19547149457073942, 2.371175808195584267 ) ) ;
#3783 = CARTESIAN_POINT ( 'NONE',  ( 7.360235569667877620, -77.25452850542924921, -0.09995255151731691212 ) ) ;
#3784 = CARTESIAN_POINT ( 'NONE',  ( -2.862020680886579349, -89.29547149457074795, -4.100960146803977580 ) ) ;
#3785 = CARTESIAN_POINT ( 'NONE',  ( -4.725907263620323207, -60.90452850542925489, 1.635492904037698647 ) ) ;
#3786 = CARTESIAN_POINT ( 'NONE',  ( -5.895805022753386027, -82.05452850542926058, 4.407101234057909878 ) ) ;
#3787 = CARTESIAN_POINT ( 'NONE',  ( 2.493201789345311337, -87.94547149457073942, 1.934965279058241006 ) ) ;
#3788 = EDGE_LOOP ( 'NONE', ( #6885, #5797, #1385, #3758 ) ) ;
#3789 = CARTESIAN_POINT ( 'NONE',  ( 0.000000000000000000, -9.999999999999994671, -30.00000000000000000 ) ) ;
#3790 = CARTESIAN_POINT ( 'NONE',  ( -3.966234939601246623, -27.25766265056033433, 4.500000000000000888 ) ) ;
#3791 = ORIENTED_EDGE ( 'NONE', *, *, #3890, .F. ) ;
#3792 = CARTESIAN_POINT ( 'NONE',  ( 5.257311121191344583, -95.25452850542926342, -0.09995255151729466603 ) ) ;
#3793 = CARTESIAN_POINT ( 'NONE',  ( 2.882544866740880174, -97.39547149457074227, -0.8366430509619593447 ) ) ;
#3794 = EDGE_CURVE ( 'NONE', #1757, #1341, #2208, .T. ) ;
#3795 = CARTESIAN_POINT ( 'NONE',  ( -1.529537955723667908, -94.35452850542922931, 5.030887037049979860 ) ) ;
#3796 = CARTESIAN_POINT ( 'NONE',  ( 6.628020296210686446, -67.09547149457073090, 2.253526892787472757 ) ) ;
#3797 = CARTESIAN_POINT ( 'NONE',  ( -1.529537955723775378, -89.14547149457074227, -5.030887037049945221 ) ) ;
#3798 = CARTESIAN_POINT ( 'NONE',  ( -2.823794231030021695, -72.90452850542925489, 1.017458915287783316 ) ) ;
#3799 = CARTESIAN_POINT ( 'NONE',  ( -5.999999999999992895, -50.00000000000000000, -2.499999999999999112 ) ) ;
#3800 = PLANE ( 'NONE',  #5832 ) ;
#3801 = CARTESIAN_POINT ( 'NONE',  ( 3.154386672714811102, -92.25452850542926342, -0.09995255151727241993 ) ) ;
#3802 = CARTESIAN_POINT ( 'NONE',  ( -4.037591185471546495, -65.29547149457073374, -5.718994135553860936 ) ) ;
#3803 = DIRECTION ( 'NONE',  ( 1.000000000000000000, 9.251858538542971581E-17, 1.604941620322696727E-32 ) ) ;
#3804 = CARTESIAN_POINT ( 'NONE',  ( 1.719659006605283702, -61.84547149457073800, -4.969112962950050338 ) ) ;
#3805 = CARTESIAN_POINT ( 'NONE',  ( 4.191402346623081421, -97.69547149457076785, -5.607243785695398941 ) ) ;
#3806 = CARTESIAN_POINT ( 'NONE',  ( -1.069819614139536190, -93.15452850542925489, -2.969112962950023249 ) ) ;
#3807 = DIRECTION ( 'NONE',  ( -1.000000000000000000, 0.000000000000000000, 0.000000000000000000 ) ) ;
#3808 = CARTESIAN_POINT ( 'NONE',  ( -4.725907263620322318, -69.90452850542925489, 1.635492904037698647 ) ) ;
#3809 = CARTESIAN_POINT ( 'NONE',  ( 5.895805022753496161, -90.94547149457073942, 4.407101234057782868 ) ) ;
#3810 = ORIENTED_EDGE ( 'NONE', *, *, #7263, .T. ) ;
#3811 = DIRECTION ( 'NONE',  ( 1.000000000000000000, 8.326672684688674053E-16, -0.000000000000000000 ) ) ;
#3812 = VECTOR ( 'NONE', #2356, 1000.000000000000000 ) ;
#3813 = SHAPE_DEFINITION_REPRESENTATION ( #1648, #1989 ) ;
#3814 = ORIENTED_EDGE ( 'NONE', *, *, #2898, .T. ) ;
#3815 = VECTOR ( 'NONE', #5130, 1000.000000000000000 ) ;
#3816 = PLANE ( 'NONE',  #853 ) ;
#3817 = CARTESIAN_POINT ( 'NONE',  ( -4.312004677471057867, -78.45452850542925205, -3.009306630940844052 ) ) ;
#3818 = CIRCLE ( 'NONE', #4761, 1.500000000000001332 ) ;
#3819 = CARTESIAN_POINT ( 'NONE',  ( 4.194503406049402194, -87.94547149457072521, 3.171033256558012159 ) ) ;
#3820 = LINE ( 'NONE', #690, #4164 ) ;
#3821 = CARTESIAN_POINT ( 'NONE',  ( -1.069819614139474906, -75.34547149457073090, 2.969112962950044121 ) ) ;
#3822 = CARTESIAN_POINT ( 'NONE',  ( 5.895805022753406455, -83.55452850542926058, -4.407101234057908989 ) ) ;
#3823 = CARTESIAN_POINT ( 'NONE',  ( -5.257311121191323267, -86.74547149457072237, -0.09995255151718371311 ) ) ;
#3824 = PLANE ( 'NONE',  #4672 ) ;
#3825 = CARTESIAN_POINT ( 'NONE',  ( -2.179377348189460939, -82.35452850542927195, 7.030887037049988741 ) ) ;
#3826 = CIRCLE ( 'NONE', #5572, 1.499999999999996225 ) ;
#3827 = CARTESIAN_POINT ( 'NONE',  ( 0.8796985632579634729, -90.64547149457075648, 3.030887037049952326 ) ) ;
#3828 = EDGE_CURVE ( 'NONE', #6779, #2259, #5400, .T. ) ;
#3829 = ORIENTED_EDGE ( 'NONE', *, *, #4472, .T. ) ;
#3830 = DIRECTION ( 'NONE',  ( 0.000000000000000000, -1.734723475976807094E-16, 1.000000000000000000 ) ) ;
#3831 = CARTESIAN_POINT ( 'NONE',  ( 55.00000000000002132, -99.99999999999998579, 20.00000000000000000 ) ) ;
#3832 = VERTEX_POINT ( 'NONE', #4764 ) ;
#3833 = CARTESIAN_POINT ( 'NONE',  ( -5.257311121191325043, -78.75452850542926342, 0.09995255151729529053 ) ) ;
#3834 = CARTESIAN_POINT ( 'NONE',  ( 1.840261337453268586, -58.80452850542926058, 2.371175808195547852 ) ) ;
#3835 = EDGE_CURVE ( 'NONE', #2966, #3118, #380, .T. ) ;
#3836 = CARTESIAN_POINT ( 'NONE',  ( 3.015831842038235955, -91.80452850542926058, 3.989209796945429432 ) ) ;
#3837 = CARTESIAN_POINT ( 'NONE',  ( 0.09506052544073349819, -70.99547149457075079, -6.999999999999997335 ) ) ;
#3838 = CARTESIAN_POINT ( 'NONE',  ( -3.015831842038128041, -84.19547149457073942, 3.989209796945492048 ) ) ;
#3839 = CARTESIAN_POINT ( 'NONE',  ( 2.610703060766983885, -73.95452850542925205, 1.773238653441072232 ) ) ;
#3840 = CARTESIAN_POINT ( 'NONE',  ( -5.108479284279210399E-14, -97.00000000000000000, -5.999999999999992006 ) ) ;
#3841 = SURFACE_STYLE_USAGE ( .BOTH. , #6873 ) ;
#3842 = CARTESIAN_POINT ( 'NONE',  ( 1.069819614139558173, -85.65452850542926910, 2.969112962950023249 ) ) ;
#3843 = CARTESIAN_POINT ( 'NONE',  ( 6.686770931921476979, -61.39547149457074937, -2.072711028461788896 ) ) ;
#3844 = CARTESIAN_POINT ( 'NONE',  ( 80.00000000000000000, 0.000000000000000000, -20.00000000000000000 ) ) ;
#3845 = CARTESIAN_POINT ( 'NONE',  ( -4.194503406049383543, -68.44547149457073942, -3.171033256558012159 ) ) ;
#3846 = CARTESIAN_POINT ( 'NONE',  ( 1.719659006605283480, -61.84547149457073090, -4.969112962950050338 ) ) ;
#3847 = CARTESIAN_POINT ( 'NONE',  ( 1.097606853890779561E-14, -87.00000000000001421, 0.000000000000000000 ) ) ;
#3848 = CARTESIAN_POINT ( 'NONE',  ( -47.50000000000000711, -97.00000000000000000, -12.50000000000002309 ) ) ;
#3849 = CARTESIAN_POINT ( 'NONE',  ( -3.015831842038216859, -63.30452850542925347, -3.989209796945429432 ) ) ;
#3850 = CARTESIAN_POINT ( 'NONE',  ( -6.686770931921458327, -86.89547149457074227, 2.072711028461789784 ) ) ;
#3851 = ORIENTED_EDGE ( 'NONE', *, *, #4049, .T. ) ;
#3852 = EDGE_CURVE ( 'NONE', #3744, #250, #2373, .T. ) ;
#3853 = DIRECTION ( 'NONE',  ( 1.000000000000000000, 0.000000000000000000, 0.000000000000000000 ) ) ;
#3854 = APPLICATION_PROTOCOL_DEFINITION ( 'draft international standard', 'automotive_design', 1998, #1309 ) ;
#3855 = VERTEX_POINT ( 'NONE', #7344 ) ;
#3856 = CARTESIAN_POINT ( 'NONE',  ( 47.49999999999998579, -88.00000000000000000, 0.000000000000000000 ) ) ;
#3857 = CARTESIAN_POINT ( 'NONE',  ( -1.719659006605372076, -75.15452850542925489, -4.969112962950016588 ) ) ;
#3858 = CARTESIAN_POINT ( 'NONE',  ( -3.015831842038128929, -78.19547149457075363, 3.989209796945492048 ) ) ;
#3859 = DIRECTION ( 'NONE',  ( -0.000000000000000000, -1.000000000000000000, -0.000000000000000000 ) ) ;
#3860 = CARTESIAN_POINT ( 'NONE',  ( 1.840261337453219292, -67.69547149457073942, -2.371175808195584267 ) ) ;
#3861 = CARTESIAN_POINT ( 'NONE',  ( 4.191402346623196884, -70.80452850542926058, 5.607243785695311900 ) ) ;
#3862 = PRODUCT_RELATED_PRODUCT_CATEGORY ( 'part', '', ( #8042 ) ) ;
#3863 = CARTESIAN_POINT ( 'NONE',  ( 2.862020680886599333, -78.79547149457074795, 4.100960146803977580 ) ) ;
#3864 = CARTESIAN_POINT ( 'NONE',  ( -1.719659006605374518, -60.15452850542926200, -4.969112962950016588 ) ) ;
#3865 = CARTESIAN_POINT ( 'NONE',  ( -1.529537955723668352, -91.35452850542921510, 5.030887037049979860 ) ) ;
#3866 = CARTESIAN_POINT ( 'NONE',  ( 6.628020296210639373, -68.40452850542925489, -2.253526892787612645 ) ) ;
#3867 = CARTESIAN_POINT ( 'NONE',  ( -2.610703060766923933, -93.04547149457074795, 1.773238653441125745 ) ) ;
#3868 = ORIENTED_EDGE ( 'NONE', *, *, #5110, .F. ) ;
#3869 = LINE ( 'NONE', #5845, #1197 ) ;
#3870 = LINE ( 'NONE', #5799, #1264 ) ;
#3871 = CARTESIAN_POINT ( 'NONE',  ( -1.529537955723668574, -88.35452850542925773, 5.030887037049979860 ) ) ;
#3872 = ORIENTED_EDGE ( 'NONE', *, *, #7477, .F. ) ;
#3873 = CARTESIAN_POINT ( 'NONE',  ( 0.09506052544086007750, -76.50452850542924921, 4.999999999999997335 ) ) ;
#3874 = CARTESIAN_POINT ( 'NONE',  ( -1.069819614139540409, -60.15452850542926200, -2.969112962950023249 ) ) ;
#3875 = SURFACE_STYLE_USAGE ( .BOTH. , #1152 ) ;
#3876 = AXIS2_PLACEMENT_3D ( 'NONE', #7856, #7176, #1402 ) ;
#3877 = CARTESIAN_POINT ( 'NONE',  ( 5.257311121191341918, -83.25452850542926342, -0.09995255151729465215 ) ) ;
#3878 = CARTESIAN_POINT ( 'NONE',  ( 6.013306294175077227, -70.54547149457074795, -4.245374608440741326 ) ) ;
#3879 = CARTESIAN_POINT ( 'NONE',  ( -5.257311121191323267, -83.74547149457075079, -0.09995255151718372699 ) ) ;
#3880 = CARTESIAN_POINT ( 'NONE',  ( -3.154386672714789341, -78.75452850542926342, 0.09995255151727280851 ) ) ;
#3881 = DIRECTION ( 'NONE',  ( -0.9954714945707483498, -0.09506052544079830746, 1.046913586349167774E-14 ) ) ;
#3882 = PLANE ( 'NONE',  #4036 ) ;
#3883 = CARTESIAN_POINT ( 'NONE',  ( 2.493201789345273589, -92.55452850542926058, -1.934965279058294518 ) ) ;
#3884 = EDGE_CURVE ( 'NONE', #1590, #7927, #797, .T. ) ;
#3885 = CARTESIAN_POINT ( 'NONE',  ( -5.895805022753479285, -65.44547149457075363, -4.407101234057782868 ) ) ;
#3886 = CARTESIAN_POINT ( 'NONE',  ( 80.00000000000000000, 2.168404344971008868E-15, -12.50000000000000000 ) ) ;
#3887 = CARTESIAN_POINT ( 'NONE',  ( 2.862020680886514956, -80.70452850542925205, -4.100960146804039752 ) ) ;
#3888 = CARTESIAN_POINT ( 'NONE',  ( -4.312004677470995695, -60.04547149457074795, 3.009306630940933758 ) ) ;
#3889 = FACE_OUTER_BOUND ( 'NONE', #7158, .T. ) ;
#3890 = EDGE_CURVE ( 'NONE', #2858, #2966, #5049, .T. ) ;
#3891 = CARTESIAN_POINT ( 'NONE',  ( 65.00000000000000000, -9.999999999999991118, -10.50000000000000888 ) ) ;
#3892 = AXIS2_PLACEMENT_3D ( 'NONE', #2818, #3487, #7243 ) ;
#3893 = CARTESIAN_POINT ( 'NONE',  ( -1.529537955723672349, -58.35452850542924352, 5.030887037049979860 ) ) ;
#3894 = CARTESIAN_POINT ( 'NONE',  ( 2.179377348189631025, -90.64547149457075648, 7.030887037049939003 ) ) ;
#3895 = ORIENTED_EDGE ( 'NONE', *, *, #6954, .T. ) ;
#3896 = AXIS2_PLACEMENT_3D ( 'NONE', #5938, #2459, #3292 ) ;
#3897 = CARTESIAN_POINT ( 'NONE',  ( -3.015831842038214639, -78.30452850542926058, -3.989209796945429432 ) ) ;
#3898 = LINE ( 'NONE', #1203, #1812 ) ;
#3899 = AXIS2_PLACEMENT_3D ( 'NONE', #5395, #2912, #6741 ) ;
#3900 = DIRECTION ( 'NONE',  ( -0.000000000000000000, -0.000000000000000000, -1.000000000000000000 ) ) ;
#3901 = CARTESIAN_POINT ( 'NONE',  ( -1.719659006605264828, -81.34547149457074511, 4.969112962950051227 ) ) ;
#3902 = DIRECTION ( 'NONE',  ( -1.000000000000000000, 0.000000000000000000, 0.000000000000000000 ) ) ;
#3903 = CARTESIAN_POINT ( 'NONE',  ( -3.154386672714790674, -71.74547149457075079, -0.09995255151720625064 ) ) ;
#3904 = CARTESIAN_POINT ( 'NONE',  ( 0.09506052544088100520, -73.50452850542924921, 6.999999999999997335 ) ) ;
#3905 = CARTESIAN_POINT ( 'NONE',  ( 45.00000000000000000, -15.00000000000000355, 9.500000000000000000 ) ) ;
#3906 = CARTESIAN_POINT ( 'NONE',  ( 4.312004677471012570, -79.54547149457074795, -3.009306630940933314 ) ) ;
#3907 = CARTESIAN_POINT ( 'NONE',  ( 3.015831842038231958, -58.80452850542925347, 3.989209796945429432 ) ) ;
#3908 = CARTESIAN_POINT ( 'NONE',  ( 5.257311121191343695, -95.25452850542924921, -0.09995255151729465215 ) ) ;
#3909 =( GEOMETRIC_REPRESENTATION_CONTEXT ( 3 ) GLOBAL_UNCERTAINTY_ASSIGNED_CONTEXT ( ( #1571 ) ) GLOBAL_UNIT_ASSIGNED_CONTEXT ( ( #2347, #3604, #4913 ) ) REPRESENTATION_CONTEXT ( 'NONE', 'WORKASPACE' ) );
#3910 = CARTESIAN_POINT ( 'NONE',  ( -2.369498399071207739, -69.15452850542926910, -6.969112962950009482 ) ) ;
#3911 = CARTESIAN_POINT ( 'NONE',  ( 1.069819614139494890, -79.84547149457074511, -2.969112962950042789 ) ) ;
#3912 = ORIENTED_EDGE ( 'NONE', *, *, #2393, .T. ) ;
#3913 = CYLINDRICAL_SURFACE ( 'NONE', #5228, 4.999999999999999112 ) ;
#3914 = CARTESIAN_POINT ( 'NONE',  ( 4.725907263620341858, -92.40452850542925489, -1.635492904037697981 ) ) ;
#3915 = CARTESIAN_POINT ( 'NONE',  ( -4.312004677471056091, -90.45452850542926626, -3.009306630940844052 ) ) ;
#3916 = VERTEX_POINT ( 'NONE', #2611 ) ;
#3917 = CARTESIAN_POINT ( 'NONE',  ( 4.312004677471078296, -79.95452850542923784, 3.009306630940844052 ) ) ;
#3918 = CARTESIAN_POINT ( 'NONE',  ( -2.882544866740878842, -63.60452850542924352, -0.8366430509618996147 ) ) ;
#3919 = DIRECTION ( 'NONE',  ( 0.000000000000000000, 0.000000000000000000, 1.000000000000000000 ) ) ;
#3920 = CARTESIAN_POINT ( 'NONE',  ( 5.257311121191342806, -86.25452850542924921, -0.09995255151729465215 ) ) ;
#3921 = CARTESIAN_POINT ( 'NONE',  ( -2.369498399071058969, -63.34547149457073800, 6.969112962950058332 ) ) ;
#3922 = EDGE_CURVE ( 'NONE', #1663, #1136, #4450, .T. ) ;
#3923 = CARTESIAN_POINT ( 'NONE',  ( -0.8796985632578808723, -64.35452850542924352, 3.030887037049973198 ) ) ;
#3924 = CARTESIAN_POINT ( 'NONE',  ( 0.09506052544075790922, -97.99547149457075079, -4.999999999999997335 ) ) ;
#3925 = CARTESIAN_POINT ( 'NONE',  ( 6.123233995736760366E-16, -27.00000000000000000, 5.000000000000000000 ) ) ;
#3926 = CARTESIAN_POINT ( 'NONE',  ( 1.686450176301586890, -89.70452850542925205, -2.482926158054133303 ) ) ;
#3927 = CARTESIAN_POINT ( 'NONE',  ( -7.360235569667860744, -65.74547149457073658, -0.09995255151716124498 ) ) ;
#3928 = LINE ( 'NONE', #5103, #4650 ) ;
#3929 = CARTESIAN_POINT ( 'NONE',  ( 1.529537955723690557, -80.85452850542925773, -5.030887037049978971 ) ) ;
#3930 = CARTESIAN_POINT ( 'NONE',  ( -4.191402346623055664, -93.19547149457075363, 5.607243785695398941 ) ) ;
#3931 = FACE_OUTER_BOUND ( 'NONE', #4353, .T. ) ;
#3932 = FACE_OUTER_BOUND ( 'NONE', #4143, .T. ) ;
#3933 = CARTESIAN_POINT ( 'NONE',  ( 2.862020680886512292, -62.70452850542926626, -4.100960146804039752 ) ) ;
#3934 = CARTESIAN_POINT ( 'NONE',  ( -6.628020296210666018, -86.59547149457075932, -2.253526892787471869 ) ) ;
#3935 = EDGE_CURVE ( 'NONE', #7792, #348, #8215, .T. ) ;
#3936 = ORIENTED_EDGE ( 'NONE', *, *, #7958, .T. ) ;
#3937 = CARTESIAN_POINT ( 'NONE',  ( 0.09506052544086007750, -76.50452850542924921, 4.999999999999997335 ) ) ;
#3938 = DIRECTION ( 'NONE',  ( 1.000000000000000000, 0.000000000000000000, 0.000000000000000000 ) ) ;
#3939 = PLANE ( 'NONE',  #5028 ) ;
#3940 = CARTESIAN_POINT ( 'NONE',  ( 4.194503406049402194, -81.94547149457073942, 3.171033256558012159 ) ) ;
#3941 = CARTESIAN_POINT ( 'NONE',  ( -0.09506052544084261924, -57.00452850542924921, -4.999999999999997335 ) ) ;
#3942 = CARTESIAN_POINT ( 'NONE',  ( -1.686450176301619308, -59.29547149457074084, -2.482926158054096000 ) ) ;
#3943 = CARTESIAN_POINT ( 'NONE',  ( -0.09506052544086251999, -66.00452850542926342, -6.999999999999997335 ) ) ;
#3944 = CARTESIAN_POINT ( 'NONE',  ( 54.99999999999999289, 80.00000000000000000, 7.500000000000000000 ) ) ;
#3945 = ADVANCED_FACE ( 'NONE', ( #7579 ), #4370, .F. ) ;
#3946 = CARTESIAN_POINT ( 'NONE',  ( 4.194503406049402194, -75.94547149457075363, 3.171033256558012159 ) ) ;
#3947 = PLANE ( 'NONE',  #1863 ) ;
#3948 = CARTESIAN_POINT ( 'NONE',  ( 1.529537955723692111, -89.85452850542925773, -5.030887037049978971 ) ) ;
#3949 = CARTESIAN_POINT ( 'NONE',  ( -4.037591185471423927, -70.20452850542925205, 5.718994135553947977 ) ) ;
#3950 = CARTESIAN_POINT ( 'NONE',  ( -3.154386672714790674, -74.74547149457073658, -0.09995255151720625064 ) ) ;
#3951 = AXIS2_PLACEMENT_3D ( 'NONE', #2780, #4832, #2150 ) ;
#3952 = VERTEX_POINT ( 'NONE', #6989 ) ;
#3953 = DIRECTION ( 'NONE',  ( 0.000000000000000000, 0.000000000000000000, 1.000000000000000000 ) ) ;
#3954 = FACE_OUTER_BOUND ( 'NONE', #6546, .T. ) ;
#3955 = CARTESIAN_POINT ( 'NONE',  ( 2.862020680886515844, -89.70452850542926626, -4.100960146804039752 ) ) ;
#3956 = ORIENTED_EDGE ( 'NONE', *, *, #4829, .T. ) ;
#3957 = CARTESIAN_POINT ( 'NONE',  ( -4.194503406049316929, -85.05452850542926058, 3.171033256558101865 ) ) ;
#3958 = CARTESIAN_POINT ( 'NONE',  ( 2.610703060766947470, -91.54547149457074795, -1.773238653441125523 ) ) ;
#3959 = DIRECTION ( 'NONE',  ( 0.8672199170124480494, -0.4979253112033197870, 0.000000000000000000 ) ) ;
#3960 = VECTOR ( 'NONE', #7779, 1000.000000000000000 ) ;
#3961 = CARTESIAN_POINT ( 'NONE',  ( -4.194503406049316041, -82.05452850542924637, 3.171033256558100533 ) ) ;
#3962 = CARTESIAN_POINT ( 'NONE',  ( -6.686770931921461880, -59.89547149457074937, 2.072711028461789784 ) ) ;
#3963 = EDGE_CURVE ( 'NONE', #6901, #2088, #6506, .T. ) ;
#3964 = CARTESIAN_POINT ( 'NONE',  ( -2.882544866740878842, -63.60452850542924352, -0.8366430509618996147 ) ) ;
#3965 = VECTOR ( 'NONE', #5376, 1000.000000000000114 ) ;
#3966 = CARTESIAN_POINT ( 'NONE',  ( 54.99999999999999289, 80.00000000000000000, 7.500000000000000000 ) ) ;
#3967 = CYLINDRICAL_SURFACE ( 'NONE', #129, 1.500000000000000666 ) ;
#3968 = CARTESIAN_POINT ( 'NONE',  ( 0.09506052544083881672, -76.50452850542926342, 2.999999999999997780 ) ) ;
#3969 = CARTESIAN_POINT ( 'NONE',  ( -5.895805022753383362, -94.05452850542926058, 4.407101234057909878 ) ) ;
#3970 = CYLINDRICAL_SURFACE ( 'NONE', #4962, 1.500000000000001998 ) ;
#3971 = CARTESIAN_POINT ( 'NONE',  ( 2.862020680886514068, -74.70452850542926626, -4.100960146804039752 ) ) ;
#3972 = CARTESIAN_POINT ( 'NONE',  ( -6.686770931921456551, -89.89547149457074227, 2.072711028461789784 ) ) ;
#3973 = DIRECTION ( 'NONE',  ( -1.000000000000000000, -0.000000000000000000, 0.000000000000000000 ) ) ;
#3974 = PLANE ( 'NONE',  #2869 ) ;
#3975 = CARTESIAN_POINT ( 'NONE',  ( 0.8796985632579613634, -72.64547149457072805, 3.030887037049952326 ) ) ;
#3976 = EDGE_CURVE ( 'NONE', #2390, #4159, #3243, .T. ) ;
#3977 = CARTESIAN_POINT ( 'NONE',  ( 4.725907263620339194, -62.40452850542925489, -1.635492904037697981 ) ) ;
#3978 = CARTESIAN_POINT ( 'NONE',  ( 2.369498399071078509, -85.84547149457074511, -6.969112962950057444 ) ) ;
#3979 = PRESENTATION_STYLE_ASSIGNMENT (( #5325 ) ) ;
#3980 = ORIENTED_EDGE ( 'NONE', *, *, #1946, .F. ) ;
#3981 = CARTESIAN_POINT ( 'NONE',  ( -2.862020680886494084, -79.20452850542925205, 4.100960146804039752 ) ) ;
#3982 = DIRECTION ( 'NONE',  ( -0.000000000000000000, -0.000000000000000000, -1.000000000000000000 ) ) ;
#3983 = CARTESIAN_POINT ( 'NONE',  ( 46.49999999999999289, -14.99999999999999467, -12.50000000000000178 ) ) ;
#3984 = CARTESIAN_POINT ( 'NONE',  ( 3.015831842038149802, -82.69547149457073942, -3.989209796945492048 ) ) ;
#3985 = CARTESIAN_POINT ( 'NONE',  ( 47.49999999999999289, -96.99999999999998579, -12.50000000000002309 ) ) ;
#3986 = CARTESIAN_POINT ( 'NONE',  ( -0.8796985632579442660, -65.14547149457074227, -3.030887037049952326 ) ) ;
#3987 = CARTESIAN_POINT ( 'NONE',  ( -7.360235569667858968, -69.75452850542926342, 0.09995255151731782806 ) ) ;
#3988 = LINE ( 'NONE', #5967, #8001 ) ;
#3989 = CARTESIAN_POINT ( 'NONE',  ( 4.784657899331177688, -79.39547149457074227, -1.454677039711874009 ) ) ;
#3990 = DIRECTION ( 'NONE',  ( 1.000000000000000000, 0.000000000000000000, 0.000000000000000000 ) ) ;
#3991 = CARTESIAN_POINT ( 'NONE',  ( 0.09506052544086160405, -88.50452850542924921, 4.999999999999997335 ) ) ;
#3992 = CARTESIAN_POINT ( 'NONE',  ( 6.013306294175167821, -64.95452850542926626, 4.245374608440616093 ) ) ;
#3993 = CARTESIAN_POINT ( 'NONE',  ( -2.493201789345290464, -77.44547149457073942, -1.934965279058240561 ) ) ;
#3994 = ORIENTED_EDGE ( 'NONE', *, *, #5256, .F. ) ;
#3995 = DIRECTION ( 'NONE',  ( -1.000000000000000000, -2.775557561562892337E-16, 0.000000000000000000 ) ) ;
#3996 = CARTESIAN_POINT ( 'NONE',  ( 4.784657899331212327, -95.10452850542925773, 1.454677039711774533 ) ) ;
#3997 = CARTESIAN_POINT ( 'NONE',  ( 0.09506052544086160405, -88.50452850542924921, 4.999999999999997335 ) ) ;
#3998 = ORIENTED_EDGE ( 'NONE', *, *, #158, .T. ) ;
#3999 = CARTESIAN_POINT ( 'NONE',  ( -4.725907263620320542, -84.90452850542925489, 1.635492904037698647 ) ) ;
#4000 = CARTESIAN_POINT ( 'NONE',  ( 1.840261337453222179, -94.69547149457076785, -2.371175808195584267 ) ) ;
#4001 = DIRECTION ( 'NONE',  ( 0.000000000000000000, 0.000000000000000000, 1.000000000000000000 ) ) ;
#4002 = CARTESIAN_POINT ( 'NONE',  ( -3.015831842038213750, -90.30452850542926058, -3.989209796945429432 ) ) ;
#4003 = CARTESIAN_POINT ( 'NONE',  ( -6.628020296210618056, -93.90452850542926910, 2.253526892787613978 ) ) ;
#4004 = CARTESIAN_POINT ( 'NONE',  ( -2.493201789345253161, -67.05452850542926058, 1.934965279058294518 ) ) ;
#4005 =( REPRESENTATION_RELATIONSHIP ('NONE','NONE', #4188, #1933 ) REPRESENTATION_RELATIONSHIP_WITH_TRANSFORMATION ( #2096 )SHAPE_REPRESENTATION_RELATIONSHIP( ) );
#4006 = CARTESIAN_POINT ( 'NONE',  ( 54.99999999999999289, -20.00000000000000000, 7.500000000000000000 ) ) ;
#4007 = PLANE ( 'NONE',  #7537 ) ;
#4008 = CARTESIAN_POINT ( 'NONE',  ( 3.154386672714809325, -80.25452850542926342, -0.09995255151727241993 ) ) ;
#4009 = CARTESIAN_POINT ( 'NONE',  ( -7.360235569667856304, -93.75452850542926342, 0.09995255151731782806 ) ) ;
#4010 = LINE ( 'NONE', #3844, #8289 ) ;
#4011 = CARTESIAN_POINT ( 'NONE',  ( 0.09506052544073539945, -85.99547149457075079, -6.999999999999997335 ) ) ;
#4012 = CARTESIAN_POINT ( 'NONE',  ( 47.49999999999998579, -82.99999999999998579, 0.000000000000000000 ) ) ;
#4013 = DIRECTION ( 'NONE',  ( -0.000000000000000000, 0.7071067811865442421, 0.7071067811865509034 ) ) ;
#4014 = CARTESIAN_POINT ( 'NONE',  ( 1.686450176301635295, -69.79547149457074795, 2.482926158054096000 ) ) ;
#4015 =( LENGTH_UNIT ( ) NAMED_UNIT ( * ) SI_UNIT ( .MILLI., .METRE. ) );
#4016 = ORIENTED_EDGE ( 'NONE', *, *, #3011, .F. ) ;
#4017 = EDGE_CURVE ( 'NONE', #1490, #7328, #2524, .T. ) ;
#4018 = CARTESIAN_POINT ( 'NONE',  ( 0.09506052544085857869, -64.50452850542926342, 4.999999999999997335 ) ) ;
#4019 = CARTESIAN_POINT ( 'NONE',  ( 4.037591185471563371, -84.79547149457074795, 5.718994135553860936 ) ) ;
#4020 = VERTEX_POINT ( 'NONE', #5672 ) ;
#4021 = CARTESIAN_POINT ( 'NONE',  ( 5.257311121191341918, -74.25452850542924921, -0.09995255151729465215 ) ) ;
#4022 = DIRECTION ( 'NONE',  ( 0.000000000000000000, 0.000000000000000000, 1.000000000000000000 ) ) ;
#4023 = EDGE_CURVE ( 'NONE', #417, #293, #6401, .T. ) ;
#4024 = ITEM_DEFINED_TRANSFORMATION ( 'NONE', 'NONE', #6585,  #2840 ) ;
#4025 = EDGE_CURVE ( 'NONE', #5382, #3327, #1300, .T. ) ;
#4026 = COLOUR_RGB ( '', 0.72549020, 0.75294118, 0.79215686) ;
#4027 = CARTESIAN_POINT ( 'NONE',  ( 1.529537955723795584, -75.64547149457069963, 5.030887037049945221 ) ) ;
#4028 = CARTESIAN_POINT ( 'NONE',  ( 65.00000000000000000, -12.00000000000000355, -12.50000000000000178 ) ) ;
#4029 = CARTESIAN_POINT ( 'NONE',  ( -0.8796985632579448211, -62.14547149457074937, -3.030887037049952326 ) ) ;
#4030 = VECTOR ( 'NONE', #6370, 1000.000000000000000 ) ;
#4031 = CARTESIAN_POINT ( 'NONE',  ( -6.628020296210620721, -72.90452850542925489, 2.253526892787613978 ) ) ;
#4032 = DIRECTION ( 'NONE',  ( 1.000000000000000000, 0.000000000000000000, 0.000000000000000000 ) ) ;
#4033 = LINE ( 'NONE', #5927, #3965 ) ;
#4034 = CARTESIAN_POINT ( 'NONE',  ( -4.194503406049316041, -82.05452850542924637, 3.171033256558100533 ) ) ;
#4035 = CARTESIAN_POINT ( 'NONE',  ( -6.013306294175152722, -66.45452850542925205, -4.245374608440613429 ) ) ;
#4036 = AXIS2_PLACEMENT_3D ( 'NONE', #2627, #4129, #4848 ) ;
#4037 = CARTESIAN_POINT ( 'NONE',  ( -2.882544866740857081, -80.89547149457074227, 0.8366430509619596778 ) ) ;
#4038 = ORIENTED_EDGE ( 'NONE', *, *, #1289, .F. ) ;
#4039 = DIRECTION ( 'NONE',  ( -0.000000000000000000, 1.000000000000000000, 2.168404344971010594E-16 ) ) ;
#4040 = CARTESIAN_POINT ( 'NONE',  ( 4.194503406049340022, -95.55452850542921794, -3.171033256558100089 ) ) ;
#4041 = CARTESIAN_POINT ( 'NONE',  ( -1.529537955723668796, -85.35452850542924352, 5.030887037049979860 ) ) ;
#4042 = ORIENTED_EDGE ( 'NONE', *, *, #6088, .F. ) ;
#4043 = CARTESIAN_POINT ( 'NONE',  ( 5.257311121191341030, -74.25452850542924921, -0.09995255151729466603 ) ) ;
#4044 = CARTESIAN_POINT ( 'NONE',  ( -1.069819614139472463, -93.34547149457073090, 2.969112962950044121 ) ) ;
#4045 = CARTESIAN_POINT ( 'NONE',  ( 1.719659006605392060, -85.65452850542922647, 4.969112962950016588 ) ) ;
#4046 = CARTESIAN_POINT ( 'NONE',  ( 2.179377348189627916, -63.64547149457072805, 7.030887037049939003 ) ) ;
#4047 = CARTESIAN_POINT ( 'NONE',  ( -0.09506052544082045641, -66.00452850542926342, -2.999999999999997780 ) ) ;
#4048 = DIRECTION ( 'NONE',  ( 1.000000000000000000, 0.000000000000000000, 0.000000000000000000 ) ) ;
#4049 = EDGE_CURVE ( 'NONE', #4845, #1012, #4494, .T. ) ;
#4050 = CARTESIAN_POINT ( 'NONE',  ( 40.00000000000000000, -9.999999999999992895, 4.499999999999999112 ) ) ;
#4051 = CARTESIAN_POINT ( 'NONE',  ( 0.09506052544083956612, -82.50452850542926342, 2.999999999999997780 ) ) ;
#4052 = CARTESIAN_POINT ( 'NONE',  ( 2.179377348189484032, -92.85452850542924352, -7.030887037049986077 ) ) ;
#4053 = CARTESIAN_POINT ( 'NONE',  ( -6.686770931921458327, -86.89547149457074227, 2.072711028461789784 ) ) ;
#4054 = DIRECTION ( 'NONE',  ( 0.000000000000000000, 1.000000000000000000, 0.000000000000000000 ) ) ;
#4055 = CARTESIAN_POINT ( 'NONE',  ( 50.00000000000000000, -7.999999999999996447, 12.49999999999999822 ) ) ;
#4056 = CARTESIAN_POINT ( 'NONE',  ( 1.069819614139492669, -64.84547149457071669, -2.969112962950042789 ) ) ;
#4057 =( NAMED_UNIT ( * ) PLANE_ANGLE_UNIT ( ) SI_UNIT ( $, .RADIAN. ) );
#4058 = VERTEX_POINT ( 'NONE', #2488 ) ;
#4059 = CARTESIAN_POINT ( 'NONE',  ( -2.862020680886495416, -70.20452850542925205, 4.100960146804039752 ) ) ;
#4060 = CARTESIAN_POINT ( 'NONE',  ( -6.013306294175060351, -78.04547149457074795, 4.245374608440741326 ) ) ;
#4061 =( NAMED_UNIT ( * ) SI_UNIT ( $, .STERADIAN. ) SOLID_ANGLE_UNIT ( ) );
#4062 = ORIENTED_EDGE ( 'NONE', *, *, #2458, .T. ) ;
#4063 = CARTESIAN_POINT ( 'NONE',  ( -4.194503406049316929, -73.05452850542926058, 3.171033256558100533 ) ) ;
#4064 = FACE_BOUND ( 'NONE', #601, .T. ) ;
#4065 = CARTESIAN_POINT ( 'NONE',  ( 1.719659006605285034, -70.84547149457074511, -4.969112962950050338 ) ) ;
#4066 = PLANE ( 'NONE',  #1348 ) ;
#4067 = CARTESIAN_POINT ( 'NONE',  ( -3.015831842038126709, -96.19547149457075363, 3.989209796945492048 ) ) ;
#4068 = CARTESIAN_POINT ( 'NONE',  ( -5.895805022753386915, -61.05452850542925347, 4.407101234057909878 ) ) ;
#4069 = PLANE ( 'NONE',  #5235 ) ;
#4070 = AXIS2_PLACEMENT_3D ( 'NONE', #4425, #7009, #1236 ) ;
#4071 = CARTESIAN_POINT ( 'NONE',  ( -80.00000000000000000, 0.000000000000000000, -20.00000000000000000 ) ) ;
#4072 = CARTESIAN_POINT ( 'NONE',  ( 4.194503406049338246, -83.55452850542921794, -3.171033256558100089 ) ) ;
#4073 = CARTESIAN_POINT ( 'NONE',  ( 6.686770931921522276, -62.10452850542925063, 2.072711028461649008 ) ) ;
#4074 = CARTESIAN_POINT ( 'NONE',  ( 1.069819614139494446, -76.84547149457073090, -2.969112962950042789 ) ) ;
#4075 = ORIENTED_EDGE ( 'NONE', *, *, #7555, .F. ) ;
#4076 = CARTESIAN_POINT ( 'NONE',  ( 80.00000000000000000, -19.99999999999999645, -12.50000000000000355 ) ) ;
#4077 = CARTESIAN_POINT ( 'NONE',  ( -5.257311121191321490, -93.75452850542926342, 0.09995255151729526277 ) ) ;
#4078 = CARTESIAN_POINT ( 'NONE',  ( 1.719659006605391394, -79.65452850542925489, 4.969112962950016588 ) ) ;
#4079 = ORIENTED_EDGE ( 'NONE', *, *, #5897, .F. ) ;
#4080 = CARTESIAN_POINT ( 'NONE',  ( 4.725907263620340082, -71.40452850542925489, -1.635492904037697981 ) ) ;
#4081 = CARTESIAN_POINT ( 'NONE',  ( 1.069819614139496666, -94.84547149457073090, -2.969112962950042789 ) ) ;
#4082 = CARTESIAN_POINT ( 'NONE',  ( 3.154386672714807105, -61.24547149457073658, 0.09995255151720662534 ) ) ;
#4083 = CARTESIAN_POINT ( 'NONE',  ( -4.191402346623176456, -93.30452850542926058, -5.607243785695311900 ) ) ;
#4084 = VECTOR ( 'NONE', #8201, 1000.000000000000000 ) ;
#4085 = CARTESIAN_POINT ( 'NONE',  ( 1.069819614139555064, -61.65452850542925489, 2.969112962950023249 ) ) ;
#4086 = EDGE_CURVE ( 'NONE', #1241, #4272, #3870, .T. ) ;
#4087 = ORIENTED_EDGE ( 'NONE', *, *, #1320, .T. ) ;
#4088 = EDGE_CURVE ( 'NONE', #943, #1587, #1984, .T. ) ;
#4089 = CARTESIAN_POINT ( 'NONE',  ( -0.09506052544084261924, -57.00452850542924921, -4.999999999999997335 ) ) ;
#4090 = DIRECTION ( 'NONE',  ( 0.000000000000000000, 0.000000000000000000, 1.000000000000000000 ) ) ;
#4091 = CARTESIAN_POINT ( 'NONE',  ( 1.686450176301586001, -80.70452850542925205, -2.482926158054133303 ) ) ;
#4092 = MECHANICAL_DESIGN_GEOMETRIC_PRESENTATION_REPRESENTATION (  '', ( #7728 ), #6103 ) ;
#4093 = CARTESIAN_POINT ( 'NONE',  ( 6.013306294175171374, -88.95452850542925205, 4.245374608440616093 ) ) ;
#4094 = VECTOR ( 'NONE', #1828, 1000.000000000000000 ) ;
#4095 = CARTESIAN_POINT ( 'NONE',  ( 6.686770931921479644, -91.39547149457074227, -2.072711028461788896 ) ) ;
#4096 = FACE_BOUND ( 'NONE', #4448, .T. ) ;
#4097 = CARTESIAN_POINT ( 'NONE',  ( 40.00000000000000000, -14.99999999999999112, 4.499999999999999112 ) ) ;
#4098 = CARTESIAN_POINT ( 'NONE',  ( -1.686450176301618642, -65.29547149457073374, -2.482926158054096000 ) ) ;
#4099 = AXIS2_PLACEMENT_3D ( 'NONE', #2269, #7016, #4392 ) ;
#4100 = DIRECTION ( 'NONE',  ( 9.251858538542972814E-17, -1.000000000000000000, 0.000000000000000000 ) ) ;
#4101 = ORIENTED_EDGE ( 'NONE', *, *, #2898, .F. ) ;
#4102 = CARTESIAN_POINT ( 'NONE',  ( 2.862020680886513624, -71.70452850542925205, -4.100960146804039752 ) ) ;
#4103 = CARTESIAN_POINT ( 'NONE',  ( -5.895805022753477509, -80.44547149457073942, -4.407101234057782868 ) ) ;
#4104 = EDGE_LOOP ( 'NONE', ( #4101, #7946, #4431, #7375, #4208 ) ) ;
#4105 = CARTESIAN_POINT ( 'NONE',  ( -1.529537955723671239, -70.35452850542925773, 5.030887037049979860 ) ) ;
#4106 = DIRECTION ( 'NONE',  ( -0.09506052544079829358, 0.9954714945707483498, 0.000000000000000000 ) ) ;
#4107 = CARTESIAN_POINT ( 'NONE',  ( 5.257311121191341918, -73.24547149457072237, 0.09995255151718437925 ) ) ;
#4108 = ADVANCED_FACE ( 'NONE', ( #5006, #6277 ), #3746, .F. ) ;
#4109 = DIRECTION ( 'NONE',  ( 0.000000000000000000, 1.000000000000000000, 2.775557561562891351E-16 ) ) ;
#4110 = CARTESIAN_POINT ( 'NONE',  ( 3.015831842038151134, -94.69547149457075363, -3.989209796945492048 ) ) ;
#4111 = CARTESIAN_POINT ( 'NONE',  ( -2.369498399071207739, -57.15452850542926200, -6.969112962950009482 ) ) ;
#4112 = EDGE_LOOP ( 'NONE', ( #5128, #304, #2148, #2467 ) ) ;
#4113 = CARTESIAN_POINT ( 'NONE',  ( -0.09506052544083960776, -81.00452850542926342, -4.999999999999997335 ) ) ;
#4114 = ORIENTED_EDGE ( 'NONE', *, *, #328, .T. ) ;
#4115 = PLANE ( 'NONE',  #2212 ) ;
#4116 = CARTESIAN_POINT ( 'NONE',  ( 1.529537955723692111, -89.85452850542925773, -5.030887037049978971 ) ) ;
#4117 = CARTESIAN_POINT ( 'NONE',  ( 2.862020680886514956, -80.70452850542925205, -4.100960146804039752 ) ) ;
#4118 = EDGE_CURVE ( 'NONE', #5910, #8028, #3160, .T. ) ;
#4119 = ORIENTED_EDGE ( 'NONE', *, *, #6196, .F. ) ;
#4120 = CARTESIAN_POINT ( 'NONE',  ( 1.719659006605390505, -73.65452850542924068, 4.969112962950015699 ) ) ;
#4121 = CARTESIAN_POINT ( 'NONE',  ( 2.823794231030061219, -88.09547149457074511, 1.017458915287723809 ) ) ;
#4122 = CARTESIAN_POINT ( 'NONE',  ( -0.09506052544073315125, -93.49547149457073658, 4.999999999999997335 ) ) ;
#4123 = CARTESIAN_POINT ( 'NONE',  ( -0.09506052544083998246, -78.00452850542926342, -4.999999999999997335 ) ) ;
#4124 = CARTESIAN_POINT ( 'NONE',  ( -7.360235569667856304, -87.75452850542924921, 0.09995255151731782806 ) ) ;
#4125 = CARTESIAN_POINT ( 'NONE',  ( 2.610703060766981665, -58.95452850542925916, 1.773238653441072232 ) ) ;
#4126 = ORIENTED_EDGE ( 'NONE', *, *, #4926, .F. ) ;
#4127 = CARTESIAN_POINT ( 'NONE',  ( 6.123233995736760366E-16, -27.00000000000000000, 2.500000000000000888 ) ) ;
#4128 = PRODUCT ( 'High-Rigidity Aluminium Body Shell', 'High-Rigidity Aluminium Body Shell', '', ( #371 ) ) ;
#4129 = DIRECTION ( 'NONE',  ( -1.000000000000000000, 0.000000000000000000, -0.000000000000000000 ) ) ;
#4130 = CARTESIAN_POINT ( 'NONE',  ( 2.882544866740896161, -74.10452850542924352, 0.8366430509618999478 ) ) ;
#4131 = CARTESIAN_POINT ( 'NONE',  ( -6.628020296210619833, -87.90452850542926910, 2.253526892787613978 ) ) ;
#4132 = CARTESIAN_POINT ( 'NONE',  ( -2.369498399071056305, -81.34547149457074511, 6.969112962950058332 ) ) ;
#4133 = PLANE ( 'NONE',  #98 ) ;
#4134 = CARTESIAN_POINT ( 'NONE',  ( -1.719659006605263274, -96.34547149457074511, 4.969112962950051227 ) ) ;
#4135 = CARTESIAN_POINT ( 'NONE',  ( -2.823794231030041235, -71.59547149457071669, -1.017458915287723364 ) ) ;
#4136 = VECTOR ( 'NONE', #1895, 1000.000000000000000 ) ;
#4137 = FACE_OUTER_BOUND ( 'NONE', #1544, .T. ) ;
#4138 = ADVANCED_FACE ( 'NONE', ( #5716 ), #8295, .T. ) ;
#4139 = ORIENTED_EDGE ( 'NONE', *, *, #7958, .F. ) ;
#4140 = PLANE ( 'NONE',  #4751 ) ;
#4141 = CARTESIAN_POINT ( 'NONE',  ( 1.529537955723689002, -65.85452850542924352, -5.030887037049978971 ) ) ;
#4142 = CARTESIAN_POINT ( 'NONE',  ( 4.191402346623078756, -76.69547149457073942, -5.607243785695398941 ) ) ;
#4143 = EDGE_LOOP ( 'NONE', ( #911, #2243, #496 ) ) ;
#4144 = CARTESIAN_POINT ( 'NONE',  ( -4.194503406049383543, -77.44547149457075363, -3.171033256558012159 ) ) ;
#4145 = CARTESIAN_POINT ( 'NONE',  ( 1.529537955723795584, -78.64547149457074227, 5.030887037049945221 ) ) ;
#4146 = CARTESIAN_POINT ( 'NONE',  ( 0.09506052544085857869, -64.50452850542926342, 4.999999999999997335 ) ) ;
#4147 = LINE ( 'NONE', #2306, #6510 ) ;
#4148 = CARTESIAN_POINT ( 'NONE',  ( 0.09506052544075488386, -73.99547149457075079, -4.999999999999997335 ) ) ;
#4149 = EDGE_CURVE ( 'NONE', #140, #3412, #4576, .T. ) ;
#4150 = CARTESIAN_POINT ( 'NONE',  ( -65.00000000000000000, -12.00000000000000711, 12.49999999999999822 ) ) ;
#4151 = CARTESIAN_POINT ( 'NONE',  ( 7.360235569667875843, -62.25452850542926342, -0.09995255151731691212 ) ) ;
#4152 = ORIENTED_EDGE ( 'NONE', *, *, #2379, .F. ) ;
#4153 = CIRCLE ( 'NONE', #2416, 1.500000000000001776 ) ;
#4154 = VERTEX_POINT ( 'NONE', #5215 ) ;
#4155 = AXIS2_PLACEMENT_3D ( 'NONE', #1061, #2535, #2076 ) ;
#4156 = CARTESIAN_POINT ( 'NONE',  ( -3.966234939601246623, -27.25766265056033433, 4.500000000000000888 ) ) ;
#4157 = CARTESIAN_POINT ( 'NONE',  ( -5.257311121191322378, -90.75452850542924921, 0.09995255151729526277 ) ) ;
#4158 = CARTESIAN_POINT ( 'NONE',  ( -1.719659006605371632, -81.15452850542922647, -4.969112962950016588 ) ) ;
#4159 = VERTEX_POINT ( 'NONE', #6649 ) ;
#4160 = CARTESIAN_POINT ( 'NONE',  ( 4.784657899331208775, -68.10452850542925773, 1.454677039711774533 ) ) ;
#4161 = CARTESIAN_POINT ( 'NONE',  ( -0.09506052544075556388, -84.49547149457075079, 2.999999999999997780 ) ) ;
#4162 = CARTESIAN_POINT ( 'NONE',  ( -2.493201789345292241, -62.44547149457074653, -1.934965279058240561 ) ) ;
#4163 = CARTESIAN_POINT ( 'NONE',  ( -2.862020680886494528, -76.20452850542926626, 4.100960146804039752 ) ) ;
#4164 = VECTOR ( 'NONE', #1290, 1000.000000000000000 ) ;
#4165 = CARTESIAN_POINT ( 'NONE',  ( -5.895805022753383362, -88.05452850542926058, 4.407101234057909878 ) ) ;
#4166 = CARTESIAN_POINT ( 'NONE',  ( -0.09506052544075442590, -93.49547149457075079, 2.999999999999997780 ) ) ;
#4167 = VERTEX_POINT ( 'NONE', #7795 ) ;
#4168 = FACE_OUTER_BOUND ( 'NONE', #1147, .T. ) ;
#4169 = ORIENTED_EDGE ( 'NONE', *, *, #2654, .T. ) ;
#4170 = DIRECTION ( 'NONE',  ( -0.000000000000000000, -0.000000000000000000, -1.000000000000000000 ) ) ;
#4171 = CARTESIAN_POINT ( 'NONE',  ( 1.686450176301584669, -71.70452850542925205, -2.482926158054133303 ) ) ;
#4172 = CARTESIAN_POINT ( 'NONE',  ( 6.686770931921525829, -89.10452850542925773, 2.072711028461649008 ) ) ;
#4173 = CARTESIAN_POINT ( 'NONE',  ( 6.013306294175077227, -76.54547149457074795, -4.245374608440741326 ) ) ;
#4174 = PLANE ( 'NONE',  #6425 ) ;
#4175 = CARTESIAN_POINT ( 'NONE',  ( 54.99999999999999289, 50.00000000000000000, -7.500000000000000000 ) ) ;
#4176 = PRESENTATION_LAYER_ASSIGNMENT (  '', '', ( #7140 ) ) ;
#4177 = CARTESIAN_POINT ( 'NONE',  ( 2.823794231030041235, -86.40452850542926910, -1.017458915287783316 ) ) ;
#4178 = PRODUCT_DEFINITION_CONTEXT ( 'detailed design', #712, 'design' ) ;
#4179 = ORIENTED_EDGE ( 'NONE', *, *, #3100, .F. ) ;
#4180 = CARTESIAN_POINT ( 'NONE',  ( 75.00000000000000000, -9.999999999999994671, 0.000000000000000000 ) ) ;
#4181 = CARTESIAN_POINT ( 'NONE',  ( 1.529537955723689224, -68.85452850542921510, -5.030887037049978971 ) ) ;
#4182 = CARTESIAN_POINT ( 'NONE',  ( -6.686770931921459216, -77.89547149457074227, 2.072711028461789784 ) ) ;
#4183 = EDGE_LOOP ( 'NONE', ( #5342, #6201, #5935, #3581 ) ) ;
#4184 = CARTESIAN_POINT ( 'NONE',  ( -4.725907263620353405, -77.59547149457074511, -1.635492904037597617 ) ) ;
#4185 = CARTESIAN_POINT ( 'NONE',  ( -4.725907263620354293, -68.59547149457073090, -1.635492904037597617 ) ) ;
#4186 = CARTESIAN_POINT ( 'NONE',  ( -5.257311121191324155, -66.75452850542923500, 0.09995255151729526277 ) ) ;
#4187 = DIRECTION ( 'NONE',  ( 0.000000000000000000, 0.000000000000000000, 1.000000000000000000 ) ) ;
#4188 = SHAPE_REPRESENTATION ( 'BR-001', ( #4828, #1201, #124, #5502, #6452, #6176, #3896, #6585, #5907, #6984, #2549, #5768, #3094, #1608 ), #6047 ) ;
#4189 = EDGE_CURVE ( 'NONE', #425, #6172, #7925, .T. ) ;
#4190 = CARTESIAN_POINT ( 'NONE',  ( -1.719659006605265716, -72.34547149457071669, 4.969112962950051227 ) ) ;
#4191 = CARTESIAN_POINT ( 'NONE',  ( -7.360235569667860744, -57.75452850542924921, 0.09995255151731782806 ) ) ;
#4192 = ORIENTED_EDGE ( 'NONE', *, *, #4808, .T. ) ;
#4193 = DIRECTION ( 'NONE',  ( 0.000000000000000000, -1.387778780781445676E-16, 1.000000000000000000 ) ) ;
#4194 = ORIENTED_EDGE ( 'NONE', *, *, #7858, .T. ) ;
#4195 = DIRECTION ( 'NONE',  ( -0.000000000000000000, 1.734723475976807094E-16, -1.000000000000000000 ) ) ;
#4196 = CARTESIAN_POINT ( 'NONE',  ( -0.09506052544083846978, -90.00452850542924921, -4.999999999999997335 ) ) ;
#4197 = CARTESIAN_POINT ( 'NONE',  ( 1.529537955723690557, -80.85452850542925773, -5.030887037049978971 ) ) ;
#4198 = VERTEX_POINT ( 'NONE', #2700 ) ;
#4199 = CARTESIAN_POINT ( 'NONE',  ( -4.725907263620322318, -66.90452850542925489, 1.635492904037698647 ) ) ;
#4200 = CARTESIAN_POINT ( 'NONE',  ( 2.493201789345310448, -81.94547149457073942, 1.934965279058241006 ) ) ;
#4201 = CARTESIAN_POINT ( 'NONE',  ( -4.312004677470991254, -93.04547149457074795, 3.009306630940933758 ) ) ;
#4202 = CARTESIAN_POINT ( 'NONE',  ( 4.784657899331208775, -65.10452850542924352, 1.454677039711774533 ) ) ;
#4203 = CARTESIAN_POINT ( 'NONE',  ( 2.179377348189483143, -86.85452850542924352, -7.030887037049986077 ) ) ;
#4204 = CARTESIAN_POINT ( 'NONE',  ( -1.069819614139472463, -93.34547149457073090, 2.969112962950044121 ) ) ;
#4205 = PRODUCT_CONTEXT ( 'NONE', #5020, 'mechanical' ) ;
#4206 = EDGE_LOOP ( 'NONE', ( #3014, #372 ) ) ;
#4207 = CARTESIAN_POINT ( 'NONE',  ( 50.00000000000000000, -9.999999999999991118, -10.50000000000000888 ) ) ;
#4208 = ORIENTED_EDGE ( 'NONE', *, *, #5375, .T. ) ;
#4209 = PLANE ( 'NONE',  #3499 ) ;
#4210 = CARTESIAN_POINT ( 'NONE',  ( 2.882544866740895717, -71.10452850542924352, 0.8366430509618999478 ) ) ;
#4211 = ADVANCED_FACE ( 'NONE', ( #7244, #3954 ), #6016, .F. ) ;
#4212 = CARTESIAN_POINT ( 'NONE',  ( 5.895805022753496161, -75.94547149457073942, 4.407101234057782868 ) ) ;
#4213 = LINE ( 'NONE', #3586, #1451 ) ;
#4214 = CARTESIAN_POINT ( 'NONE',  ( 4.725907263620374721, -94.09547149457074511, 1.635492904037598283 ) ) ;
#4215 = CARTESIAN_POINT ( 'NONE',  ( 1.069819614139558617, -88.65452850542926910, 2.969112962950023249 ) ) ;
#4216 = COLOUR_RGB ( '', 0.40784314, 0.44705882, 0.49803922) ;
#4217 = CARTESIAN_POINT ( 'NONE',  ( 47.49999999999999289, -49.99999999999998579, 12.49999999999993960 ) ) ;
#4218 = CIRCLE ( 'NONE', #1674, 3.000000000000000000 ) ;
#4219 = ORIENTED_EDGE ( 'NONE', *, *, #2281, .T. ) ;
#4220 = CARTESIAN_POINT ( 'NONE',  ( -0.7729879516809968765, -24.10129518119626013, 4.500000000000000888 ) ) ;
#4221 = CARTESIAN_POINT ( 'NONE',  ( -4.725907263620324095, -57.90452850542925489, 1.635492904037698647 ) ) ;
#4222 = CARTESIAN_POINT ( 'NONE',  ( 4.037591185471560706, -66.79547149457073374, 5.718994135553860936 ) ) ;
#4223 = EDGE_CURVE ( 'NONE', #6872, #4020, #748, .T. ) ;
#4224 =( LENGTH_UNIT ( ) NAMED_UNIT ( * ) SI_UNIT ( .MILLI., .METRE. ) );
#4225 = ORIENTED_EDGE ( 'NONE', *, *, #4086, .F. ) ;
#4226 = CARTESIAN_POINT ( 'NONE',  ( 4.784657899331177688, -76.39547149457074227, -1.454677039711874009 ) ) ;
#4227 = CARTESIAN_POINT ( 'NONE',  ( 3.015831842038147581, -67.69547149457073942, -3.989209796945492048 ) ) ;
#4228 = CIRCLE ( 'NONE', #3556, 1.500000000000000666 ) ;
#4229 = CARTESIAN_POINT ( 'NONE',  ( 4.194503406049334693, -62.55452850542925347, -3.171033256558100089 ) ) ;
#4230 = LINE ( 'NONE', #3519, #2617 ) ;
#4231 = VECTOR ( 'NONE', #7834, 1000.000000000000000 ) ;
#4232 = CARTESIAN_POINT ( 'NONE',  ( 4.725907263620371168, -64.09547149457073090, 1.635492904037598283 ) ) ;
#4233 = SURFACE_SIDE_STYLE ('',( #1670 ) ) ;
#4234 = CARTESIAN_POINT ( 'NONE',  ( 5.257311121191343695, -95.25452850542924921, -0.09995255151729465215 ) ) ;
#4235 = ORIENTED_EDGE ( 'NONE', *, *, #842, .T. ) ;
#4236 = DIRECTION ( 'NONE',  ( 0.000000000000000000, -1.000000000000000000, -2.775557561562891351E-16 ) ) ;
#4237 = EDGE_CURVE ( 'NONE', #1673, #4574, #2190, .T. ) ;
#4238 = ORIENTED_EDGE ( 'NONE', *, *, #6316, .T. ) ;
#4239 = CARTESIAN_POINT ( 'NONE',  ( -80.00000000000000000, -2.168404344971008868E-15, 12.50000000000000000 ) ) ;
#4240 = CARTESIAN_POINT ( 'NONE',  ( 4.312004677471076519, -82.95452850542925205, 3.009306630940844496 ) ) ;
#4241 = CARTESIAN_POINT ( 'NONE',  ( 4.312004677471075631, -73.95452850542926626, 3.009306630940844496 ) ) ;
#4242 = CARTESIAN_POINT ( 'NONE',  ( 2.862020680886512292, -62.70452850542926626, -4.100960146804039752 ) ) ;
#4243 = CARTESIAN_POINT ( 'NONE',  ( 3.154386672714809770, -79.24547149457073658, 0.09995255151720662534 ) ) ;
#4244 = CARTESIAN_POINT ( 'NONE',  ( 4.784657899331179465, -94.39547149457074227, -1.454677039711874009 ) ) ;
#4245 = CARTESIAN_POINT ( 'NONE',  ( 0.09506052544085932809, -70.50452850542926342, 4.999999999999997335 ) ) ;
#4246 = CARTESIAN_POINT ( 'NONE',  ( -0.09506052544086027178, -84.00452850542926342, -6.999999999999997335 ) ) ;
#4247 = CARTESIAN_POINT ( 'NONE',  ( 1.069819614139554842, -58.65452850542925489, 2.969112962950023249 ) ) ;
#4248 = ITEM_DEFINED_TRANSFORMATION ( 'NONE', 'NONE', #124,  #2840 ) ;
#4249 = ORIENTED_EDGE ( 'NONE', *, *, #4189, .F. ) ;
#4250 = DIRECTION ( 'NONE',  ( 0.000000000000000000, 0.000000000000000000, -1.000000000000000000 ) ) ;
#4251 = CARTESIAN_POINT ( 'NONE',  ( 3.015831842038235511, -88.80452850542926058, 3.989209796945429432 ) ) ;
#4252 = CARTESIAN_POINT ( 'NONE',  ( -0.8796985632578796510, -73.35452850542924352, 3.030887037049973198 ) ) ;
#4253 = CARTESIAN_POINT ( 'NONE',  ( 6.628020296210687334, -76.09547149457073090, 2.253526892787472757 ) ) ;
#4254 = CARTESIAN_POINT ( 'NONE',  ( -4.725907263620318766, -93.90452850542925489, 1.635492904037698647 ) ) ;
#4255 = CARTESIAN_POINT ( 'NONE',  ( -2.862020680886578905, -92.29547149457074795, -4.100960146803977580 ) ) ;
#4256 = CARTESIAN_POINT ( 'NONE',  ( -2.493201789345250496, -88.05452850542926058, 1.934965279058294518 ) ) ;
#4257 = PLANE ( 'NONE',  #4155 ) ;
#4258 = ORIENTED_EDGE ( 'NONE', *, *, #5762, .T. ) ;
#4259 = LINE ( 'NONE', #8029, #7458 ) ;
#4260 = CARTESIAN_POINT ( 'NONE',  ( -1.719659006605374518, -60.15452850542926200, -4.969112962950016588 ) ) ;
#4261 = CARTESIAN_POINT ( 'NONE',  ( -4.191402346623058328, -69.19547149457073942, 5.607243785695398941 ) ) ;
#4262 = CARTESIAN_POINT ( 'NONE',  ( 0.5177642813940753763, -97.00000000000001421, -5.999999999999999112 ) ) ;
#4263 = CARTESIAN_POINT ( 'NONE',  ( -3.015831842038129373, -75.19547149457073942, 3.989209796945492048 ) ) ;
#4264 = CARTESIAN_POINT ( 'NONE',  ( -4.194503406049384431, -65.44547149457072521, -3.171033256558012159 ) ) ;
#4265 = CARTESIAN_POINT ( 'NONE',  ( -2.882544866740875733, -90.60452850542925773, -0.8366430509618996147 ) ) ;
#4266 = DIRECTION ( 'NONE',  ( -1.000000000000000000, 0.000000000000000000, 0.000000000000000000 ) ) ;
#4267 = ADVANCED_FACE ( 'NONE', ( #5259 ), #3414, .T. ) ;
#4268 =( REPRESENTATION_RELATIONSHIP ('NONE','NONE', #4188, #153 ) REPRESENTATION_RELATIONSHIP_WITH_TRANSFORMATION ( #7825 )SHAPE_REPRESENTATION_RELATIONSHIP( ) );
#4269 = CARTESIAN_POINT ( 'NONE',  ( -5.257311121191324155, -59.74547149457072948, -0.09995255151718371311 ) ) ;
#4270 = VECTOR ( 'NONE', #5817, 1000.000000000000000 ) ;
#4271 = CARTESIAN_POINT ( 'NONE',  ( -5.257311121191321490, -93.75452850542926342, 0.09995255151729526277 ) ) ;
#4272 = VERTEX_POINT ( 'NONE', #5887 ) ;
#4273 = EDGE_CURVE ( 'NONE', #5032, #4887, #1801, .T. ) ;
#4274 = UNCERTAINTY_MEASURE_WITH_UNIT (LENGTH_MEASURE( 1.000000000000000082E-05 ), #2414, 'distance_accuracy_value', 'NONE');
#4275 = FACE_OUTER_BOUND ( 'NONE', #1014, .T. ) ;
#4276 = EDGE_LOOP ( 'NONE', ( #8174, #6317, #4791, #1080 ) ) ;
#4277 = CARTESIAN_POINT ( 'NONE',  ( 80.00000000000000000, -7.999999999999996447, 12.49999999999999822 ) ) ;
#4278 = CARTESIAN_POINT ( 'NONE',  ( -1.719659006605370744, -87.15452850542926910, -4.969112962950016588 ) ) ;
#4279 = CARTESIAN_POINT ( 'NONE',  ( 2.862020680886600665, -87.79547149457074795, 4.100960146803977580 ) ) ;
#4280 = CARTESIAN_POINT ( 'NONE',  ( -2.862020680886496304, -61.20452850542925205, 4.100960146804039752 ) ) ;
#4281 = CARTESIAN_POINT ( 'NONE',  ( 1.069819614139494890, -79.84547149457074511, -2.969112962950042789 ) ) ;
#4282 = CARTESIAN_POINT ( 'NONE',  ( 2.862020680886601109, -90.79547149457074795, 4.100960146803977580 ) ) ;
#4283 = CARTESIAN_POINT ( 'NONE',  ( 1.529537955723689002, -65.85452850542924352, -5.030887037049978971 ) ) ;
#4284 = CARTESIAN_POINT ( 'NONE',  ( -0.09506052544085988321, -87.00452850542926342, -6.999999999999997335 ) ) ;
#4285 = CARTESIAN_POINT ( 'NONE',  ( 2.882544866740880174, -97.39547149457074227, -0.8366430509619593447 ) ) ;
#4286 = VECTOR ( 'NONE', #3303, 1000.000000000000000 ) ;
#4287 = AXIS2_PLACEMENT_3D ( 'NONE', #8294, #3830, #1983 ) ;
#4288 = ORIENTED_EDGE ( 'NONE', *, *, #3379, .F. ) ;
#4289 = DIRECTION ( 'NONE',  ( -1.000000000000000000, 0.000000000000000000, -0.000000000000000000 ) ) ;
#4290 = ORIENTED_EDGE ( 'NONE', *, *, #414, .F. ) ;
#4291 = CARTESIAN_POINT ( 'NONE',  ( 4.312004677471078296, -94.95452850542926626, 3.009306630940844052 ) ) ;
#4292 = CARTESIAN_POINT ( 'NONE',  ( 2.610703060766982553, -64.95452850542926626, 1.773238653441072232 ) ) ;
#4293 = CARTESIAN_POINT ( 'NONE',  ( -2.882544866740855749, -95.89547149457075648, 0.8366430509619596778 ) ) ;
#4294 = CARTESIAN_POINT ( 'NONE',  ( -6.628020296210666018, -83.59547149457075932, -2.253526892787471869 ) ) ;
#4295 = CARTESIAN_POINT ( 'NONE',  ( 4.194503406049340022, -95.55452850542921794, -3.171033256558100089 ) ) ;
#4296 = CARTESIAN_POINT ( 'NONE',  ( 4.312004677471013459, -91.54547149457074795, -3.009306630940932425 ) ) ;
#4297 = CARTESIAN_POINT ( 'NONE',  ( 2.610703060766984773, -85.95452850542925205, 1.773238653441072232 ) ) ;
#4298 = AXIS2_PLACEMENT_3D ( 'NONE', #212, #2327, #6697 ) ;
#4299 =( NAMED_UNIT ( * ) PLANE_ANGLE_UNIT ( ) SI_UNIT ( $, .RADIAN. ) );
#4300 = ORIENTED_EDGE ( 'NONE', *, *, #1781, .F. ) ;
#4301 = CARTESIAN_POINT ( 'NONE',  ( -0.9662349396012467340, -27.25766265056033433, 2.500000000000000888 ) ) ;
#4302 = CARTESIAN_POINT ( 'NONE',  ( -2.610703060766962569, -93.45452850542926626, -1.773238653441072232 ) ) ;
#4303 = CARTESIAN_POINT ( 'NONE',  ( -2.179377348189612373, -68.14547149457074227, -7.030887037049939003 ) ) ;
#4304 = CARTESIAN_POINT ( 'NONE',  ( 5.646814530099427465, -96.99999999999992895, 0.2111776093032153578 ) ) ;
#4305 = CARTESIAN_POINT ( 'NONE',  ( 5.257311121191341030, -70.24547149457076500, 0.09995255151718437925 ) ) ;
#4306 = CARTESIAN_POINT ( 'NONE',  ( -4.784657899331159037, -71.89547149457074227, 1.454677039711874675 ) ) ;
#4307 = CARTESIAN_POINT ( 'NONE',  ( -5.257311121191324155, -57.75452850542923500, 0.09995255151729526277 ) ) ;
#4308 = DIRECTION ( 'NONE',  ( -0.000000000000000000, -8.673617379884033007E-17, -1.000000000000000000 ) ) ;
#4309 = CARTESIAN_POINT ( 'NONE',  ( -1.719659006605372964, -72.15452850542921226, -4.969112962950016588 ) ) ;
#4310 = CARTESIAN_POINT ( 'NONE',  ( 1.719659006605283480, -61.84547149457073090, -4.969112962950050338 ) ) ;
#4311 =( NAMED_UNIT ( * ) SI_UNIT ( $, .STERADIAN. ) SOLID_ANGLE_UNIT ( ) );
#4312 = ORIENTED_EDGE ( 'NONE', *, *, #2637, .F. ) ;
#4313 = LINE ( 'NONE', #7488, #8010 ) ;
#4314 = ORIENTED_EDGE ( 'NONE', *, *, #4992, .F. ) ;
#4315 = DIRECTION ( 'NONE',  ( -0.000000000000000000, -0.000000000000000000, -1.000000000000000000 ) ) ;
#4316 = CARTESIAN_POINT ( 'NONE',  ( 3.015831842038233734, -73.80452850542926058, 3.989209796945429432 ) ) ;
#4317 = CARTESIAN_POINT ( 'NONE',  ( -5.257311121191322378, -92.74547149457073658, -0.09995255151718371311 ) ) ;
#4318 = CARTESIAN_POINT ( 'NONE',  ( 5.257311121191341030, -59.25452850542924921, -0.09995255151729466603 ) ) ;
#4319 = CARTESIAN_POINT ( 'NONE',  ( -3.154386672714789785, -77.74547149457073658, -0.09995255151720625064 ) ) ;
#4320 = CARTESIAN_POINT ( 'NONE',  ( 6.686770931921524941, -83.10452850542927195, 2.072711028461649008 ) ) ;
#4321 = CARTESIAN_POINT ( 'NONE',  ( -4.725907263620352516, -83.59547149457074511, -1.635492904037597617 ) ) ;
#4322 = CARTESIAN_POINT ( 'NONE',  ( 0.09506052544085857869, -64.50452850542926342, 4.999999999999997335 ) ) ;
#4323 = CARTESIAN_POINT ( 'NONE',  ( -4.191402346623179120, -78.30452850542926058, -5.607243785695311900 ) ) ;
#4324 = CARTESIAN_POINT ( 'NONE',  ( 1.840261337453221957, -91.69547149457075363, -2.371175808195584267 ) ) ;
#4325 = ORIENTED_EDGE ( 'NONE', *, *, #6898, .F. ) ;
#4326 = DIRECTION ( 'NONE',  ( -0.000000000000000000, -0.000000000000000000, 1.000000000000000000 ) ) ;
#4327 = ORIENTED_EDGE ( 'NONE', *, *, #1405, .T. ) ;
#4328 = CARTESIAN_POINT ( 'NONE',  ( -4.194503406049316041, -91.05452850542924637, 3.171033256558101865 ) ) ;
#4329 = CARTESIAN_POINT ( 'NONE',  ( -1.069819614139539521, -69.15452850542926910, -2.969112962950023249 ) ) ;
#4330 = CARTESIAN_POINT ( 'NONE',  ( 6.013306294175167821, -58.95452850542925916, 4.245374608440616093 ) ) ;
#4331 = CARTESIAN_POINT ( 'NONE',  ( 4.037591185471560706, -66.79547149457073374, 5.718994135553860936 ) ) ;
#4332 = CARTESIAN_POINT ( 'NONE',  ( -2.862020680886492308, -94.20452850542926626, 4.100960146804039752 ) ) ;
#4333 = ADVANCED_FACE ( 'NONE', ( #2819 ), #5960, .T. ) ;
#4334 = AXIS2_PLACEMENT_3D ( 'NONE', #2504, #5066, #6377 ) ;
#4335 = CARTESIAN_POINT ( 'NONE',  ( -4.194503406049381766, -89.44547149457073942, -3.171033256558012159 ) ) ;
#4336 = CARTESIAN_POINT ( 'NONE',  ( -1.686450176301564685, -85.20452850542925205, 2.482926158054133303 ) ) ;
#4337 = DIRECTION ( 'NONE',  ( -0.000000000000000000, 0.000000000000000000, 1.000000000000000000 ) ) ;
#4338 = ORIENTED_EDGE ( 'NONE', *, *, #2919, .F. ) ;
#4339 = FACE_OUTER_BOUND ( 'NONE', #7117, .T. ) ;
#4340 = CARTESIAN_POINT ( 'NONE',  ( -1.069819614139536190, -93.15452850542925489, -2.969112962950023249 ) ) ;
#4341 = CARTESIAN_POINT ( 'NONE',  ( -5.895805022753479285, -71.44547149457072521, -4.407101234057782868 ) ) ;
#4342 = CARTESIAN_POINT ( 'NONE',  ( 0.000000000000000000, 0.000000000000000000, 0.000000000000000000 ) ) ;
#4343 = DIRECTION ( 'NONE',  ( -1.000000000000000000, 0.000000000000000000, -0.000000000000000000 ) ) ;
#4344 = CARTESIAN_POINT ( 'NONE',  ( 4.194503406049400418, -63.94547149457074653, 3.171033256558012159 ) ) ;
#4345 = CARTESIAN_POINT ( 'NONE',  ( 4.312004677471010794, -64.54547149457073374, -3.009306630940933314 ) ) ;
#4346 = CARTESIAN_POINT ( 'NONE',  ( -1.719659006605374518, -60.15452850542926200, -4.969112962950016588 ) ) ;
#4347 = LINE ( 'NONE', #7727, #4737 ) ;
#4348 = AXIS2_PLACEMENT_3D ( 'NONE', #5756, #3200, #7624 ) ;
#4349 = AXIS2_PLACEMENT_3D ( 'NONE', #8125, #8241, #1718 ) ;
#4350 = CARTESIAN_POINT ( 'NONE',  ( -3.015831842038215527, -72.30452850542926058, -3.989209796945429432 ) ) ;
#4351 = CARTESIAN_POINT ( 'NONE',  ( -3.015831842038131150, -60.19547149457074653, 3.989209796945492048 ) ) ;
#4352 = AXIS2_PLACEMENT_3D ( 'NONE', #1710, #5535, #3600 ) ;
#4353 = EDGE_LOOP ( 'NONE', ( #1507, #4713, #4770, #4863, #2489, #7500, #3936, #5279, #2268, #1302 ) ) ;
#4354 = AXIS2_PLACEMENT_3D ( 'NONE', #8108, #4902, #7474 ) ;
#4355 = FACE_OUTER_BOUND ( 'NONE', #7998, .T. ) ;
#4356 =( GEOMETRIC_REPRESENTATION_CONTEXT ( 3 ) GLOBAL_UNCERTAINTY_ASSIGNED_CONTEXT ( ( #3016 ) ) GLOBAL_UNIT_ASSIGNED_CONTEXT ( ( #7238, #1546, #7917 ) ) REPRESENTATION_CONTEXT ( 'NONE', 'WORKASPACE' ) );
#4357 = ORIENTED_EDGE ( 'NONE', *, *, #3828, .F. ) ;
#4358 = CARTESIAN_POINT ( 'NONE',  ( 75.00000000000000000, 1.301042606982605715E-15, -7.500000000000002665 ) ) ;
#4359 = CARTESIAN_POINT ( 'NONE',  ( -4.194503406049316929, -73.05452850542926058, 3.171033256558100533 ) ) ;
#4360 = CARTESIAN_POINT ( 'NONE',  ( 0.09506052544075677124, -88.99547149457073658, -4.999999999999997335 ) ) ;
#4361 = CARTESIAN_POINT ( 'NONE',  ( 1.719659006605389395, -64.65452850542925489, 4.969112962950015699 ) ) ;
#4362 = CARTESIAN_POINT ( 'NONE',  ( 2.493201789345309560, -72.94547149457073942, 1.934965279058241006 ) ) ;
#4363 = CARTESIAN_POINT ( 'NONE',  ( 7.360235569667878508, -80.25452850542926342, -0.09995255151731691212 ) ) ;
#4364 = CARTESIAN_POINT ( 'NONE',  ( -4.725907263620351628, -92.59547149457074511, -1.635492904037597617 ) ) ;
#4365 = CARTESIAN_POINT ( 'NONE',  ( -1.719659006605372964, -72.15452850542921226, -4.969112962950016588 ) ) ;
#4366 = CARTESIAN_POINT ( 'NONE',  ( 4.191402346623197772, -73.80452850542926058, 5.607243785695311900 ) ) ;
#4367 = CARTESIAN_POINT ( 'NONE',  ( 2.823794231030061219, -88.09547149457074511, 1.017458915287723809 ) ) ;
#4368 = ORIENTED_EDGE ( 'NONE', *, *, #7634, .F. ) ;
#4369 = CARTESIAN_POINT ( 'NONE',  ( 65.00000000000000000, -7.999999999999996447, 12.49999999999999822 ) ) ;
#4370 = PLANE ( 'NONE',  #4614 ) ;
#4371 = ORIENTED_EDGE ( 'NONE', *, *, #2976, .F. ) ;
#4372 = CARTESIAN_POINT ( 'NONE',  ( -0.09506052544083808120, -93.00452850542926342, -4.999999999999997335 ) ) ;
#4373 = CARTESIAN_POINT ( 'NONE',  ( -2.493201789345254049, -61.05452850542925347, 1.934965279058294518 ) ) ;
#4374 = CARTESIAN_POINT ( 'NONE',  ( -0.09506052544083770650, -96.00452850542926342, -4.999999999999997335 ) ) ;
#4375 = CARTESIAN_POINT ( 'NONE',  ( -2.369498399071058969, -66.34547149457073090, 6.969112962950058332 ) ) ;
#4376 = CARTESIAN_POINT ( 'NONE',  ( -4.312004677470992142, -84.04547149457074795, 3.009306630940933314 ) ) ;
#4377 = CARTESIAN_POINT ( 'NONE',  ( -0.8796985632578788739, -79.35452850542927195, 3.030887037049973198 ) ) ;
#4378 = MANIFOLD_SOLID_BREP ( 'Boss-Extrude4', #5181 ) ;
#4379 = ADVANCED_BREP_SHAPE_REPRESENTATION ( '', ( #7177, #2840 ), #5779 ) ;
#4380 = ADVANCED_FACE ( 'NONE', ( #303 ), #4513, .F. ) ;
#4381 = ORIENTED_EDGE ( 'NONE', *, *, #5622, .F. ) ;
#4382 = CARTESIAN_POINT ( 'NONE',  ( 4.194503406049334693, -59.55452850542926058, -3.171033256558100089 ) ) ;
#4383 = CARTESIAN_POINT ( 'NONE',  ( 2.369498399071075845, -67.84547149457071669, -6.969112962950057444 ) ) ;
#4384 = CARTESIAN_POINT ( 'NONE',  ( -47.50000000000000711, -46.99999999999998579, 12.49999999999999112 ) ) ;
#4385 = CARTESIAN_POINT ( 'NONE',  ( 3.015831842038146693, -61.69547149457073942, -3.989209796945492048 ) ) ;
#4386 = CARTESIAN_POINT ( 'NONE',  ( -2.862020680886582458, -59.29547149457074084, -4.100960146803977580 ) ) ;
#4387 = CARTESIAN_POINT ( 'NONE',  ( -2.862020680886496748, -58.20452850542925916, 4.100960146804039752 ) ) ;
#4388 = CARTESIAN_POINT ( 'NONE',  ( 55.00000000000000000, -25.00000000000002132, -20.00000000000000000 ) ) ;
#4389 = CARTESIAN_POINT ( 'NONE',  ( 4.784657899331208775, -71.10452850542925773, 1.454677039711774533 ) ) ;
#4390 = CARTESIAN_POINT ( 'NONE',  ( -4.312004677470995695, -60.04547149457074795, 3.009306630940933758 ) ) ;
#4391 = ORIENTED_EDGE ( 'NONE', *, *, #1776, .F. ) ;
#4392 = DIRECTION ( 'NONE',  ( 1.000000000000000000, 0.000000000000000000, 0.000000000000000000 ) ) ;
#4393 = EDGE_CURVE ( 'NONE', #7734, #4681, #1572, .T. ) ;
#4394 = VERTEX_POINT ( 'NONE', #5361 ) ;
#4395 = PLANE ( 'NONE',  #7317 ) ;
#4396 = CARTESIAN_POINT ( 'NONE',  ( -4.725907263620320542, -81.90452850542925489, 1.635492904037698647 ) ) ;
#4397 = CARTESIAN_POINT ( 'NONE',  ( 4.194503406049402194, -93.94547149457075363, 3.171033256558012159 ) ) ;
#4398 = CARTESIAN_POINT ( 'NONE',  ( -4.194503406049321370, -58.05452850542925347, 3.171033256558101865 ) ) ;
#4399 = CARTESIAN_POINT ( 'NONE',  ( 0.8796985632579618075, -75.64547149457072805, 3.030887037049952326 ) ) ;
#4400 = CARTESIAN_POINT ( 'NONE',  ( -6.013306294175150946, -81.45452850542925205, -4.245374608440613429 ) ) ;
#4401 = CARTESIAN_POINT ( 'NONE',  ( 4.725907263620374721, -88.09547149457074511, 1.635492904037598283 ) ) ;
#4402 = LINE ( 'NONE', #6981, #4136 ) ;
#4403 = CARTESIAN_POINT ( 'NONE',  ( -2.369498399071206851, -75.15452850542922647, -6.969112962950009482 ) ) ;
#4404 = CARTESIAN_POINT ( 'NONE',  ( 1.069819614139495556, -85.84547149457074511, -2.969112962950042789 ) ) ;
#4405 = EDGE_LOOP ( 'NONE', ( #4753, #1982, #4238, #5633 ) ) ;
#4406 = DIRECTION ( 'NONE',  ( -0.000000000000000000, -0.000000000000000000, -1.000000000000000000 ) ) ;
#4407 = CARTESIAN_POINT ( 'NONE',  ( -4.725907263620356069, -59.59547149457074511, -1.635492904037597617 ) ) ;
#4408 = ORIENTED_EDGE ( 'NONE', *, *, #359, .F. ) ;
#4409 = CARTESIAN_POINT ( 'NONE',  ( 1.529537955723692111, -89.85452850542925773, -5.030887037049978971 ) ) ;
#4410 = CARTESIAN_POINT ( 'NONE',  ( -1.840261337453254153, -57.30452850542924637, -2.371175808195547852 ) ) ;
#4411 = CARTESIAN_POINT ( 'NONE',  ( 6.628020296210639373, -59.40452850542925489, -2.253526892787612645 ) ) ;
#4412 = CARTESIAN_POINT ( 'NONE',  ( 6.628020296210686446, -73.09547149457071669, 2.253526892787472757 ) ) ;
#4413 = AXIS2_PLACEMENT_3D ( 'NONE', #4369, #7541, #8214 ) ;
#4414 = CARTESIAN_POINT ( 'NONE',  ( 2.862020680886600221, -84.79547149457074795, 4.100960146803977580 ) ) ;
#4415 = CARTESIAN_POINT ( 'NONE',  ( -2.610703060766965233, -75.45452850542925205, -1.773238653441072232 ) ) ;
#4416 = CARTESIAN_POINT ( 'NONE',  ( 54.99999999999999289, 1.301042606982605715E-15, -7.500000000000002665 ) ) ;
#4417 = SURFACE_STYLE_FILL_AREA ( #1102 ) ;
#4418 = CARTESIAN_POINT ( 'NONE',  ( 2.610703060766986106, -91.95452850542925205, 1.773238653441072232 ) ) ;
#4419 = VECTOR ( 'NONE', #713, 1000.000000000000000 ) ;
#4420 = CARTESIAN_POINT ( 'NONE',  ( 2.369498399071075401, -61.84547149457074511, -6.969112962950057444 ) ) ;
#4421 = CARTESIAN_POINT ( 'NONE',  ( 65.00000000000000000, -9.999999999999991118, -10.50000000000000888 ) ) ;
#4422 = CARTESIAN_POINT ( 'NONE',  ( 4.194503406049400418, -60.94547149457073232, 3.171033256558012159 ) ) ;
#4423 = CARTESIAN_POINT ( 'NONE',  ( 2.369498399071080286, -97.84547149457073090, -6.969112962950057444 ) ) ;
#4424 = CARTESIAN_POINT ( 'NONE',  ( 2.862020680886511848, -59.70452850542925205, -4.100960146804039752 ) ) ;
#4425 = CARTESIAN_POINT ( 'NONE',  ( 6.123233995736760366E-16, -26.99999999999998934, -7.000000000000000000 ) ) ;
#4426 = CIRCLE ( 'NONE', #4840, 1.500000000000001776 ) ;
#4427 = CARTESIAN_POINT ( 'NONE',  ( -1.719659006605373408, -69.15452850542924068, -4.969112962950016588 ) ) ;
#4428 = MANIFOLD_SOLID_BREP ( 'Boss-Extrude1', #5039 ) ;
#4429 = COLOUR_RGB ( '', 0.08235294, 0.09019608, 0.10196078) ;
#4430 = CARTESIAN_POINT ( 'NONE',  ( -6.628020296210665130, -89.59547149457074511, -2.253526892787471869 ) ) ;
#4431 = ORIENTED_EDGE ( 'NONE', *, *, #2789, .T. ) ;
#4432 = CARTESIAN_POINT ( 'NONE',  ( 50.00000000000000000, -7.999999999999992895, -12.50000000000000178 ) ) ;
#4433 = ADVANCED_FACE ( 'NONE', ( #8066 ), #980, .F. ) ;
#4434 = PRESENTATION_LAYER_ASSIGNMENT (  '', '', ( #4854 ) ) ;
#4435 = ADVANCED_FACE ( 'NONE', ( #4137 ), #852, .F. ) ;
#4436 = ITEM_DEFINED_TRANSFORMATION ( 'NONE', 'NONE', #1201,  #2840 ) ;
#4437 = EDGE_LOOP ( 'NONE', ( #4357, #3198, #1176, #3590 ) ) ;
#4438 = PLANE ( 'NONE',  #5968 ) ;
#4439 = CARTESIAN_POINT ( 'NONE',  ( -4.194503406049316041, -82.05452850542924637, 3.171033256558100533 ) ) ;
#4440 = CARTESIAN_POINT ( 'NONE',  ( 2.862020680886601554, -93.79547149457074795, 4.100960146803977580 ) ) ;
#4441 = CARTESIAN_POINT ( 'NONE',  ( 4.266483400374380786, -96.99999999999998579, 2.517034344952451264 ) ) ;
#4442 = CARTESIAN_POINT ( 'NONE',  ( -3.154386672714791118, -68.74547149457075079, -0.09995255151720625064 ) ) ;
#4443 = CARTESIAN_POINT ( 'NONE',  ( 2.369498399071225947, -82.65452850542926910, 6.969112962950009482 ) ) ;
#4444 = CARTESIAN_POINT ( 'NONE',  ( 5.257311121191342806, -91.24547149457072237, 0.09995255151718437925 ) ) ;
#4445 = CARTESIAN_POINT ( 'NONE',  ( 75.00000000000000000, 1.040834085586084848E-15, -7.500000000000003553 ) ) ;
#4446 = CARTESIAN_POINT ( 'NONE',  ( 2.369498399071225947, -82.65452850542926910, 6.969112962950009482 ) ) ;
#4447 = CARTESIAN_POINT ( 'NONE',  ( -1.840261337453198864, -90.19547149457073942, 2.371175808195584267 ) ) ;
#4448 = EDGE_LOOP ( 'NONE', ( #6609, #986, #4194, #6804 ) ) ;
#4449 = CARTESIAN_POINT ( 'NONE',  ( -80.00000000000000000, -2.168404344971008868E-15, 12.50000000000000000 ) ) ;
#4450 = LINE ( 'NONE', #6439, #8259 ) ;
#4451 = ORIENTED_EDGE ( 'NONE', *, *, #1793, .T. ) ;
#4452 = CARTESIAN_POINT ( 'NONE',  ( 1.719659006605391616, -82.65452850542925489, 4.969112962950015699 ) ) ;
#4453 = CARTESIAN_POINT ( 'NONE',  ( 2.493201789345312669, -96.94547149457073942, 1.934965279058241006 ) ) ;
#4454 = CARTESIAN_POINT ( 'NONE',  ( -5.895805022753386915, -58.05452850542925347, 4.407101234057909878 ) ) ;
#4455 = CARTESIAN_POINT ( 'NONE',  ( 2.179377348189629249, -72.64547149457072805, 7.030887037049939003 ) ) ;
#4456 = CARTESIAN_POINT ( 'NONE',  ( 1.719659006605286811, -85.84547149457075932, -4.969112962950050338 ) ) ;
#4457 = CARTESIAN_POINT ( 'NONE',  ( 0.09506052544083919142, -79.50452850542926342, 2.999999999999997780 ) ) ;
#4458 = MANIFOLD_SOLID_BREP ( 'Boss-Extrude1', #1148 ) ;
#4459 = LINE ( 'NONE', #6535, #2690 ) ;
#4460 = ADVANCED_FACE ( 'NONE', ( #7303 ), #6705, .T. ) ;
#4461 = DIRECTION ( 'NONE',  ( -1.000000000000000000, 0.000000000000000000, 0.000000000000000000 ) ) ;
#4462 = CARTESIAN_POINT ( 'NONE',  ( 2.882544866740898382, -92.10452850542925773, 0.8366430509618999478 ) ) ;
#4463 = CARTESIAN_POINT ( 'NONE',  ( -2.369498399071058969, -63.34547149457073800, 6.969112962950058332 ) ) ;
#4464 = VECTOR ( 'NONE', #5690, 1000.000000000000114 ) ;
#4465 = CARTESIAN_POINT ( 'NONE',  ( 50.00000000000000000, -9.999999999999994671, 1.500000000000000666 ) ) ;
#4466 = PRODUCT_DEFINITION_SHAPE ( 'NONE', 'NONE',  #8346 ) ;
#4467 = CARTESIAN_POINT ( 'NONE',  ( 1.719659006605284590, -67.84547149457071669, -4.969112962950050338 ) ) ;
#4468 = CARTESIAN_POINT ( 'NONE',  ( -3.015831842038131150, -60.19547149457074653, 3.989209796945492048 ) ) ;
#4469 = FACE_OUTER_BOUND ( 'NONE', #2160, .T. ) ;
#4470 = CARTESIAN_POINT ( 'NONE',  ( 50.00000000000000000, -9.999999999999991118, -10.50000000000000888 ) ) ;
#4471 = CARTESIAN_POINT ( 'NONE',  ( 3.015831842038232846, -67.80452850542926058, 3.989209796945429432 ) ) ;
#4472 = EDGE_CURVE ( 'NONE', #6658, #2655, #5486, .T. ) ;
#4473 = CARTESIAN_POINT ( 'NONE',  ( 7.360235569667880284, -88.24547149457073658, 0.09995255151716216091 ) ) ;
#4474 = ORIENTED_EDGE ( 'NONE', *, *, #2117, .T. ) ;
#4475 = DIRECTION ( 'NONE',  ( -0.000000000000000000, 2.775557561562891351E-16, -1.000000000000000000 ) ) ;
#4476 = CIRCLE ( 'NONE', #4349, 0.9999999999999948930 ) ;
#4477 = APPLICATION_PROTOCOL_DEFINITION ( 'draft international standard', 'automotive_design', 1998, #3030 ) ;
#4478 = ORIENTED_EDGE ( 'NONE', *, *, #328, .F. ) ;
#4479 = CARTESIAN_POINT ( 'NONE',  ( -1.500000000000000666, -26.99999999999998934, 0.000000000000000000 ) ) ;
#4480 = CARTESIAN_POINT ( 'NONE',  ( -0.09506052544083960776, -81.00452850542926342, -4.999999999999997335 ) ) ;
#4481 = CARTESIAN_POINT ( 'NONE',  ( 4.194503406049402194, -78.94547149457071100, 3.171033256558012159 ) ) ;
#4482 = PLANE ( 'NONE',  #6462 ) ;
#4483 = CARTESIAN_POINT ( 'NONE',  ( -0.8796985632579439329, -68.14547149457074227, -3.030887037049952326 ) ) ;
#4484 = CARTESIAN_POINT ( 'NONE',  ( 2.179377348189480479, -65.85452850542924352, -7.030887037049986077 ) ) ;
#4485 = CARTESIAN_POINT ( 'NONE',  ( 4.312004677471012570, -76.54547149457071953, -3.009306630940933314 ) ) ;
#4486 = CARTESIAN_POINT ( 'NONE',  ( 4.194503406049334693, -62.55452850542925347, -3.171033256558100089 ) ) ;
#4487 = ADVANCED_FACE ( 'NONE', ( #2375 ), #1187, .F. ) ;
#4488 = DIRECTION ( 'NONE',  ( -9.251858538542971581E-17, 1.000000000000000000, -0.000000000000000000 ) ) ;
#4489 = CARTESIAN_POINT ( 'NONE',  ( 6.628020296210641149, -77.40452850542925489, -2.253526892787612645 ) ) ;
#4490 = VECTOR ( 'NONE', #270, 1000.000000000000000 ) ;
#4491 = CARTESIAN_POINT ( 'NONE',  ( 2.610703060766947470, -91.54547149457074795, -1.773238653441125523 ) ) ;
#4492 = ORIENTED_EDGE ( 'NONE', *, *, #5753, .T. ) ;
#4493 = CARTESIAN_POINT ( 'NONE',  ( 75.00000000000000000, -1.301042606982604729E-15, 7.499999999999997335 ) ) ;
#4494 = LINE ( 'NONE', #1941, #994 ) ;
#4495 = CARTESIAN_POINT ( 'NONE',  ( 4.784657899331211439, -89.10452850542925773, 1.454677039711774533 ) ) ;
#4496 = EDGE_LOOP ( 'NONE', ( #4139, #2006, #2486, #6056 ) ) ;
#4497 = CARTESIAN_POINT ( 'NONE',  ( 4.312004677471076519, -76.95452850542925205, 3.009306630940844052 ) ) ;
#4498 = CARTESIAN_POINT ( 'NONE',  ( 1.686450176301583337, -59.70452850542925916, -2.482926158054133303 ) ) ;
#4499 = ADVANCED_FACE ( 'NONE', ( #2453 ), #466, .F. ) ;
#4500 = CARTESIAN_POINT ( 'NONE',  ( 0.09506052544086160405, -88.50452850542924921, 4.999999999999997335 ) ) ;
#4501 = CARTESIAN_POINT ( 'NONE',  ( -4.037591185471546495, -65.29547149457073374, -5.718994135553860936 ) ) ;
#4502 = CARTESIAN_POINT ( 'NONE',  ( 0.09506052544075677124, -88.99547149457073658, -4.999999999999997335 ) ) ;
#4503 = CARTESIAN_POINT ( 'NONE',  ( 1.840261337453271251, -79.80452850542926058, 2.371175808195547852 ) ) ;
#4504 = DIRECTION ( 'NONE',  ( 1.000000000000000000, 0.000000000000000000, 0.000000000000000000 ) ) ;
#4505 = DIRECTION ( 'NONE',  ( 0.000000000000000000, -2.775557561562891351E-16, 1.000000000000000000 ) ) ;
#4506 = CARTESIAN_POINT ( 'NONE',  ( -2.823794231030019031, -90.90452850542926910, 1.017458915287783316 ) ) ;
#4507 = CARTESIAN_POINT ( 'NONE',  ( -2.369498399071059414, -60.34547149457074511, 6.969112962950058332 ) ) ;
#4508 = DIRECTION ( 'NONE',  ( 0.000000000000000000, 1.000000000000000000, -1.734723475976806108E-16 ) ) ;
#4509 = CARTESIAN_POINT ( 'NONE',  ( -1.719659006605266827, -69.34547149457073090, 4.969112962950051227 ) ) ;
#4510 = CARTESIAN_POINT ( 'NONE',  ( 7.360235569667880284, -97.24547149457075079, 0.09995255151716216091 ) ) ;
#4511 = DIRECTION ( 'NONE',  ( 1.000000000000000000, 0.000000000000000000, 0.000000000000000000 ) ) ;
#4512 = PLANE ( 'NONE',  #1518 ) ;
#4513 = PLANE ( 'NONE',  #3426 ) ;
#4514 = CARTESIAN_POINT ( 'NONE',  ( 0.09506052544073574639, -88.99547149457075079, -6.999999999999997335 ) ) ;
#4515 =( LENGTH_UNIT ( ) NAMED_UNIT ( * ) SI_UNIT ( .MILLI., .METRE. ) );
#4516 = ORIENTED_EDGE ( 'NONE', *, *, #3043, .F. ) ;
#4517 = CARTESIAN_POINT ( 'NONE',  ( 4.312004677471075631, -73.95452850542926626, 3.009306630940844496 ) ) ;
#4518 = LINE ( 'NONE', #1242, #190 ) ;
#4519 = ADVANCED_FACE ( 'NONE', ( #504 ), #5725, .F. ) ;
#4520 = LINE ( 'NONE', #7101, #42 ) ;
#4521 = CARTESIAN_POINT ( 'NONE',  ( -5.257311121191324155, -80.74547149457075079, -0.09995255151718371311 ) ) ;
#4522 = EDGE_CURVE ( 'NONE', #2390, #3622, #4937, .T. ) ;
#4523 = CARTESIAN_POINT ( 'NONE',  ( 2.322632124362881356, -96.99999999999992895, -3.314508707690180689 ) ) ;
#4524 = CARTESIAN_POINT ( 'NONE',  ( -2.610703060766926153, -75.04547149457074795, 1.773238653441125745 ) ) ;
#4525 = CARTESIAN_POINT ( 'NONE',  ( -6.686770931921506289, -72.60452850542924352, -2.072711028461647675 ) ) ;
#4526 = DIRECTION ( 'NONE',  ( 0.6099942813304201072, 0.7924058156930603447, 0.000000000000000000 ) ) ;
#4527 = CARTESIAN_POINT ( 'NONE',  ( -3.015831842038128485, -81.19547149457073942, 3.989209796945492048 ) ) ;
#4528 = CARTESIAN_POINT ( 'NONE',  ( -4.194503406049320482, -61.05452850542923926, 3.171033256558100533 ) ) ;
#4529 = CARTESIAN_POINT ( 'NONE',  ( -4.194503406049315153, -91.05452850542923215, 3.171033256558100533 ) ) ;
#4530 = CARTESIAN_POINT ( 'NONE',  ( 4.037591185471441690, -65.70452850542925205, -5.718994135553947977 ) ) ;
#4531 = CARTESIAN_POINT ( 'NONE',  ( -1.840261337453200641, -75.19547149457073942, 2.371175808195584267 ) ) ;
#4532 = ORIENTED_EDGE ( 'NONE', *, *, #2742, .T. ) ;
#4533 = CARTESIAN_POINT ( 'NONE',  ( 1.097606853890779561E-14, -87.00000000000001421, 0.000000000000000000 ) ) ;
#4534 = CARTESIAN_POINT ( 'NONE',  ( -2.862020680886582458, -59.29547149457074084, -4.100960146803977580 ) ) ;
#4535 = CARTESIAN_POINT ( 'NONE',  ( 1.719659006605392060, -85.65452850542922647, 4.969112962950016588 ) ) ;
#4536 = ORIENTED_EDGE ( 'NONE', *, *, #2230, .F. ) ;
#4537 = CARTESIAN_POINT ( 'NONE',  ( -3.015831842038214639, -78.30452850542926058, -3.989209796945429432 ) ) ;
#4538 = CARTESIAN_POINT ( 'NONE',  ( 3.154386672714811990, -97.24547149457075079, 0.09995255151720662534 ) ) ;
#4539 = CARTESIAN_POINT ( 'NONE',  ( -5.257311121191322378, -90.75452850542924921, 0.09995255151729526277 ) ) ;
#4540 = CARTESIAN_POINT ( 'NONE',  ( 0.09506052544073198551, -58.99547149457073658, -6.999999999999997335 ) ) ;
#4541 = CARTESIAN_POINT ( 'NONE',  ( -2.862020680886580237, -80.29547149457074795, -4.100960146803977580 ) ) ;
#4542 = CARTESIAN_POINT ( 'NONE',  ( 2.882544866740896161, -74.10452850542924352, 0.8366430509618999478 ) ) ;
#4543 = MANIFOLD_SOLID_BREP ( 'Cut-Extrude2', #1549 ) ;
#4544 = LINE ( 'NONE', #3966, #4419 ) ;
#4545 = DIRECTION ( 'NONE',  ( -1.000000000000000000, 0.000000000000000000, 0.000000000000000000 ) ) ;
#4546 = CARTESIAN_POINT ( 'NONE',  ( -2.882544866740876177, -84.60452850542927195, -0.8366430509618996147 ) ) ;
#4547 = CARTESIAN_POINT ( 'NONE',  ( 6.013306294175172262, -94.95452850542926626, 4.245374608440616093 ) ) ;
#4548 = CARTESIAN_POINT ( 'NONE',  ( 80.00000000000000000, -9.999999999999994671, 1.500000000000000666 ) ) ;
#4549 = CARTESIAN_POINT ( 'NONE',  ( 4.725907263620340082, -77.40452850542925489, -1.635492904037697981 ) ) ;
#4550 = CARTESIAN_POINT ( 'NONE',  ( 2.862020680886598001, -63.79547149457074084, 4.100960146803977580 ) ) ;
#4551 = CARTESIAN_POINT ( 'NONE',  ( 6.000000000000006217, -47.00000000000000000, 2.500000000000000888 ) ) ;
#4552 = DIRECTION ( 'NONE',  ( 0.000000000000000000, 1.000000000000000000, 0.000000000000000000 ) ) ;
#4553 = AXIS2_PLACEMENT_3D ( 'NONE', #2871, #5350, #6780 ) ;
#4554 = CARTESIAN_POINT ( 'NONE',  ( 0.09506052544085819012, -61.50452850542925631, 4.999999999999997335 ) ) ;
#4555 = EDGE_CURVE ( 'NONE', #3832, #2974, #1701, .T. ) ;
#4556 = CARTESIAN_POINT ( 'NONE',  ( 4.191402346623080533, -88.69547149457073942, -5.607243785695398941 ) ) ;
#4557 = EDGE_LOOP ( 'NONE', ( #4038, #4536, #2743, #7635 ) ) ;
#4558 = CARTESIAN_POINT ( 'NONE',  ( 3.015831842038234178, -79.80452850542926058, 3.989209796945429432 ) ) ;
#4559 = CARTESIAN_POINT ( 'NONE',  ( -0.09506052544084034328, -75.00452850542924921, -4.999999999999997335 ) ) ;
#4560 = DIRECTION ( 'NONE',  ( -0.000000000000000000, 1.000000000000000000, 2.775557561562891351E-16 ) ) ;
#4561 = AXIS2_PLACEMENT_3D ( 'NONE', #1541, #273, #3521 ) ;
#4562 = DIRECTION ( 'NONE',  ( 0.000000000000000000, 1.000000000000000000, 0.000000000000000000 ) ) ;
#4563 = CARTESIAN_POINT ( 'NONE',  ( 3.015831842038148913, -76.69547149457075363, -3.989209796945492048 ) ) ;
#4564 = CARTESIAN_POINT ( 'NONE',  ( 0.000000000000000000, -9.999999999999994671, -30.00000000000000000 ) ) ;
#4565 = CARTESIAN_POINT ( 'NONE',  ( 3.154386672714807105, -61.24547149457073658, 0.09995255151720662534 ) ) ;
#4566 = CARTESIAN_POINT ( 'NONE',  ( 6.686770931921523164, -71.10452850542924352, 2.072711028461649008 ) ) ;
#4567 = DIRECTION ( 'NONE',  ( 0.7924058156930603447, -0.6099942813304201072, 0.000000000000000000 ) ) ;
#4568 = CARTESIAN_POINT ( 'NONE',  ( 4.312004677471013459, -82.54547149457074795, -3.009306630940933314 ) ) ;
#4569 = CARTESIAN_POINT ( 'NONE',  ( 4.725907263620339194, -59.40452850542926200, -1.635492904037697981 ) ) ;
#4570 = CARTESIAN_POINT ( 'NONE',  ( 4.194503406049339134, -89.55452850542926058, -3.171033256558100089 ) ) ;
#4571 = PRESENTATION_LAYER_ASSIGNMENT (  '', '', ( #1216 ) ) ;
#4572 = CARTESIAN_POINT ( 'NONE',  ( 6.013306294175168709, -67.95452850542925205, 4.245374608440616093 ) ) ;
#4573 = CARTESIAN_POINT ( 'NONE',  ( 2.493201789345310004, -75.94547149457073942, 1.934965279058241006 ) ) ;
#4574 = VERTEX_POINT ( 'NONE', #4416 ) ;
#4575 = FACE_OUTER_BOUND ( 'NONE', #1632, .T. ) ;
#4576 = LINE ( 'NONE', #6566, #3684 ) ;
#4577 = CARTESIAN_POINT ( 'NONE',  ( -2.862020680886493196, -85.20452850542925205, 4.100960146804039752 ) ) ;
#4578 = ORIENTED_EDGE ( 'NONE', *, *, #7335, .F. ) ;
#4579 = CARTESIAN_POINT ( 'NONE',  ( 4.312004677471078296, -85.95452850542926626, 3.009306630940844052 ) ) ;
#4580 = CARTESIAN_POINT ( 'NONE',  ( 1.069819614139496000, -91.84547149457074511, -2.969112962950042789 ) ) ;
#4581 = CARTESIAN_POINT ( 'NONE',  ( -31.55601659751036081, 8.414937759336110545, -6.999999999999999112 ) ) ;
#4582 = CARTESIAN_POINT ( 'NONE',  ( 4.784657899331211439, -86.10452850542925773, 1.454677039711774533 ) ) ;
#4583 = ADVANCED_FACE ( 'NONE', ( #424 ), #548, .T. ) ;
#4584 = CARTESIAN_POINT ( 'NONE',  ( -6.628020296210668683, -62.59547149457074511, -2.253526892787471869 ) ) ;
#4585 = CARTESIAN_POINT ( 'NONE',  ( -2.493201789345253605, -64.05452850542924637, 1.934965279058294518 ) ) ;
#4586 = DIRECTION ( 'NONE',  ( 1.000000000000000000, 0.000000000000000000, 0.000000000000000000 ) ) ;
#4587 = DIRECTION ( 'NONE',  ( 1.000000000000000000, 0.000000000000000000, 0.000000000000000000 ) ) ;
#4588 = CARTESIAN_POINT ( 'NONE',  ( -1.840261337453250823, -84.30452850542926058, -2.371175808195547852 ) ) ;
#4589 = CARTESIAN_POINT ( 'NONE',  ( -2.179377348189459163, -94.35452850542925773, 7.030887037049988741 ) ) ;
#4590 = EDGE_CURVE ( 'NONE', #1162, #1663, #5681, .T. ) ;
#4591 = DIRECTION ( 'NONE',  ( 0.000000000000000000, -1.734723475976806108E-16, -1.000000000000000000 ) ) ;
#4592 = CARTESIAN_POINT ( 'NONE',  ( 4.725907263620340970, -80.40452850542925489, -1.635492904037697981 ) ) ;
#4593 = CARTESIAN_POINT ( 'NONE',  ( -6.013306294175058575, -87.04547149457074795, 4.245374608440741326 ) ) ;
#4594 = CYLINDRICAL_SURFACE ( 'NONE', #1584, 4.000000000000000000 ) ;
#4595 = CARTESIAN_POINT ( 'NONE',  ( -54.99999999999999289, -97.00000000000000000, 20.00000000000000000 ) ) ;
#4596 = CARTESIAN_POINT ( 'NONE',  ( 1.840261337453219515, -70.69547149457073942, -2.371175808195584267 ) ) ;
#4597 = CARTESIAN_POINT ( 'NONE',  ( -4.312004677471061420, -57.45452850542925916, -3.009306630940844052 ) ) ;
#4598 = CARTESIAN_POINT ( 'NONE',  ( -2.179377348189609265, -86.14547149457072805, -7.030887037049939003 ) ) ;
#4599 =( NAMED_UNIT ( * ) PLANE_ANGLE_UNIT ( ) SI_UNIT ( $, .RADIAN. ) );
#4600 = EDGE_LOOP ( 'NONE', ( #6668, #8043, #1076, #5565 ) ) ;
#4601 = CARTESIAN_POINT ( 'NONE',  ( 1.719659006605391394, -79.65452850542925489, 4.969112962950016588 ) ) ;
#4602 = DIRECTION ( 'NONE',  ( 1.000000000000000000, 0.000000000000000000, 0.000000000000000000 ) ) ;
#4603 = CARTESIAN_POINT ( 'NONE',  ( 75.00000000000000000, -30.00000000000000000, 7.499999999999992006 ) ) ;
#4604 = CARTESIAN_POINT ( 'NONE',  ( 5.257311121191341918, -79.24547149457075079, 0.09995255151718437925 ) ) ;
#4605 = DIRECTION ( 'NONE',  ( -0.000000000000000000, -0.000000000000000000, 1.000000000000000000 ) ) ;
#4606 = CARTESIAN_POINT ( 'NONE',  ( 2.823794231030057666, -61.09547149457074511, 1.017458915287723809 ) ) ;
#4607 = CARTESIAN_POINT ( 'NONE',  ( 5.895805022753406455, -74.55452850542926058, -4.407101234057908989 ) ) ;
#4608 = CARTESIAN_POINT ( 'NONE',  ( -80.00000000000000000, 0.000000000000000000, 20.00000000000000000 ) ) ;
#4609 = CARTESIAN_POINT ( 'NONE',  ( -3.015831842038129373, -75.19547149457073942, 3.989209796945492048 ) ) ;
#4610 =( NAMED_UNIT ( * ) PLANE_ANGLE_UNIT ( ) SI_UNIT ( $, .RADIAN. ) );
#4611 = CARTESIAN_POINT ( 'NONE',  ( -1.529537955723668574, -88.35452850542925773, 5.030887037049979860 ) ) ;
#4612 = CARTESIAN_POINT ( 'NONE',  ( 2.179377348189481367, -71.85452850542924352, -7.030887037049986077 ) ) ;
#4613 = CARTESIAN_POINT ( 'NONE',  ( -2.823794231030039903, -80.59547149457075932, -1.017458915287723364 ) ) ;
#4614 = AXIS2_PLACEMENT_3D ( 'NONE', #3117, #5173, #6945 ) ;
#4615 = AXIS2_PLACEMENT_3D ( 'NONE', #2685, #1326, #8323 ) ;
#4616 = AXIS2_PLACEMENT_3D ( 'NONE', #7786, #1375, #740 ) ;
#4617 = VERTEX_POINT ( 'NONE', #8147 ) ;
#4618 = CARTESIAN_POINT ( 'NONE',  ( -80.00000000000000000, -25.00000000000000000, 20.00000000000000000 ) ) ;
#4619 = CARTESIAN_POINT ( 'NONE',  ( -1.529537955723667908, -94.35452850542922931, 5.030887037049979860 ) ) ;
#4620 = CARTESIAN_POINT ( 'NONE',  ( 4.312004677471078296, -85.95452850542925205, 3.009306630940844496 ) ) ;
#4621 = VERTEX_POINT ( 'NONE', #6200 ) ;
#4622 = CARTESIAN_POINT ( 'NONE',  ( -0.09506052544083960776, -81.00452850542926342, -4.999999999999997335 ) ) ;
#4623 = CARTESIAN_POINT ( 'NONE',  ( -2.823794231030038571, -92.59547149457074511, -1.017458915287723364 ) ) ;
#4624 = CARTESIAN_POINT ( 'NONE',  ( 80.00000000000000000, 0.000000000000000000, 0.000000000000000000 ) ) ;
#4625 = VECTOR ( 'NONE', #4266, 1000.000000000000000 ) ;
#4626 = CARTESIAN_POINT ( 'NONE',  ( -3.015831842038213750, -87.30452850542926058, -3.989209796945429432 ) ) ;
#4627 = CARTESIAN_POINT ( 'NONE',  ( -0.09506052544071605381, -60.49547149457073658, 6.999999999999997335 ) ) ;
#4628 = CARTESIAN_POINT ( 'NONE',  ( 3.154386672714807105, -62.25452850542926342, -0.09995255151727241993 ) ) ;
#4629 = EDGE_CURVE ( 'NONE', #184, #1772, #8265, .T. ) ;
#4630 = AXIS2_PLACEMENT_3D ( 'NONE', #1078, #8041, #5542 ) ;
#4631 = CARTESIAN_POINT ( 'NONE',  ( 45.96623493960122886, -14.74233734943963192, 4.500000000000000888 ) ) ;
#4632 = DIRECTION ( 'NONE',  ( -0.2576626505603331063, 0.9662349396012461789, 0.000000000000000000 ) ) ;
#4633 = CARTESIAN_POINT ( 'NONE',  ( -2.493201789345251829, -79.05452850542926058, 1.934965279058294518 ) ) ;
#4634 = CARTESIAN_POINT ( 'NONE',  ( -4.191402346623177344, -90.30452850542926058, -5.607243785695311900 ) ) ;
#4635 = EDGE_CURVE ( 'NONE', #7734, #4394, #3125, .T. ) ;
#4636 = DIRECTION ( 'NONE',  ( 0.000000000000000000, -0.7071067811865507924, 0.7071067811865441310 ) ) ;
#4637 = CARTESIAN_POINT ( 'NONE',  ( 6.628020296210689111, -91.09547149457074511, 2.253526892787472757 ) ) ;
#4638 = CARTESIAN_POINT ( 'NONE',  ( 50.00000000000000000, -19.99999999999999645, -7.500000000000006217 ) ) ;
#4639 = PLANE ( 'NONE',  #1131 ) ;
#4640 = CARTESIAN_POINT ( 'NONE',  ( 1.686450176301635517, -72.79547149457074795, 2.482926158054096000 ) ) ;
#4641 = EDGE_CURVE ( 'NONE', #4887, #5032, #395, .T. ) ;
#4642 = CARTESIAN_POINT ( 'NONE',  ( 5.257311121191341918, -62.25452850542924921, -0.09995255151729465215 ) ) ;
#4643 = ORIENTED_EDGE ( 'NONE', *, *, #6814, .T. ) ;
#4644 = CARTESIAN_POINT ( 'NONE',  ( -4.784657899331190123, -72.60452850542925773, -1.454677039711773867 ) ) ;
#4645 = CARTESIAN_POINT ( 'NONE',  ( 7.360235569667877620, -76.24547149457073658, 0.09995255151716216091 ) ) ;
#4646 = SURFACE_SIDE_STYLE ('',( #225 ) ) ;
#4647 = VERTEX_POINT ( 'NONE', #3169 ) ;
#4648 = CARTESIAN_POINT ( 'NONE',  ( -4.194503406049316929, -76.05452850542926058, 3.171033256558100533 ) ) ;
#4649 = LINE ( 'NONE', #4687, #1676 ) ;
#4650 = VECTOR ( 'NONE', #6496, 1000.000000000000000 ) ;
#4651 = CARTESIAN_POINT ( 'NONE',  ( -0.09506052544073503863, -78.49547149457073658, 4.999999999999997335 ) ) ;
#4652 = CARTESIAN_POINT ( 'NONE',  ( 47.50000000000002132, -54.00000000000000711, -12.50000000000001954 ) ) ;
#4653 = CARTESIAN_POINT ( 'NONE',  ( -2.882544866740859746, -62.89547149457074227, 0.8366430509619596778 ) ) ;
#4654 = CARTESIAN_POINT ( 'NONE',  ( 0.09506052544088061662, -70.50452850542926342, 6.999999999999997335 ) ) ;
#4655 = CARTESIAN_POINT ( 'NONE',  ( -3.999999999999988898, -87.00000000000001421, 4.898587196589413815E-16 ) ) ;
#4656 = CARTESIAN_POINT ( 'NONE',  ( -4.194503406049384431, -74.44547149457071100, -3.171033256558012159 ) ) ;
#4657 = CARTESIAN_POINT ( 'NONE',  ( -0.09506052544083921918, -84.00452850542926342, -4.999999999999997335 ) ) ;
#4658 = CARTESIAN_POINT ( 'NONE',  ( -2.369498399071207739, -66.15452850542925489, -6.969112962950009482 ) ) ;
#4659 = CARTESIAN_POINT ( 'NONE',  ( 1.069819614139495112, -82.84547149457074511, -2.969112962950042789 ) ) ;
#4660 = ADVANCED_FACE ( 'NONE', ( #8303 ), #4257, .F. ) ;
#4661 = ORIENTED_EDGE ( 'NONE', *, *, #4023, .F. ) ;
#4662 = DIRECTION ( 'NONE',  ( -0.000000000000000000, 0.000000000000000000, -1.000000000000000000 ) ) ;
#4663 = CARTESIAN_POINT ( 'NONE',  ( -4.725907263620318766, -93.90452850542925489, 1.635492904037698647 ) ) ;
#4664 = CARTESIAN_POINT ( 'NONE',  ( 5.257311121191342806, -92.25452850542922079, -0.09995255151729465215 ) ) ;
#4665 = ORIENTED_EDGE ( 'NONE', *, *, #4223, .F. ) ;
#4666 = CARTESIAN_POINT ( 'NONE',  ( 0.09506052544085971667, -73.50452850542924921, 4.999999999999997335 ) ) ;
#4667 = CARTESIAN_POINT ( 'NONE',  ( 0.8796985632579631398, -87.64547149457075648, 3.030887037049952326 ) ) ;
#4668 = CARTESIAN_POINT ( 'NONE',  ( -4.784657899331189235, -87.60452850542925773, -1.454677039711773867 ) ) ;
#4669 = CARTESIAN_POINT ( 'NONE',  ( 2.179377348189484476, -95.85452850542924352, -7.030887037049986077 ) ) ;
#4670 = CARTESIAN_POINT ( 'NONE',  ( 2.610703060766983441, -70.95452850542925205, 1.773238653441072232 ) ) ;
#4671 = DIRECTION ( 'NONE',  ( 0.000000000000000000, 0.7071067811865507924, 0.7071067811865441310 ) ) ;
#4672 = AXIS2_PLACEMENT_3D ( 'NONE', #613, #3194, #6558 ) ;
#4673 = DIRECTION ( 'NONE',  ( 1.000000000000000000, 0.000000000000000000, 0.000000000000000000 ) ) ;
#4674 = CARTESIAN_POINT ( 'NONE',  ( -2.493201789345251385, -82.05452850542926058, 1.934965279058294518 ) ) ;
#4675 = CARTESIAN_POINT ( 'NONE',  ( -4.037591185471422150, -85.20452850542925205, 5.718994135553947977 ) ) ;
#4676 = CARTESIAN_POINT ( 'NONE',  ( -0.09506052544071266763, -87.49547149457075079, 6.999999999999997335 ) ) ;
#4677 = LINE ( 'NONE', #7381, #2932 ) ;
#4678 = CARTESIAN_POINT ( 'NONE',  ( 50.00000000000000000, -9.999999999999994671, -1.500000000000000666 ) ) ;
#4679 = CARTESIAN_POINT ( 'NONE',  ( -2.610703060766926598, -72.04547149457074795, 1.773238653441125745 ) ) ;
#4680 =( NAMED_UNIT ( * ) SI_UNIT ( $, .STERADIAN. ) SOLID_ANGLE_UNIT ( ) );
#4681 = VERTEX_POINT ( 'NONE', #2711 ) ;
#4682 = CARTESIAN_POINT ( 'NONE',  ( 1.719659006605389839, -70.65452850542926910, 4.969112962950016588 ) ) ;
#4683 = CARTESIAN_POINT ( 'NONE',  ( 7.360235569667877620, -79.24547149457073658, 0.09995255151716216091 ) ) ;
#4684 =( LENGTH_UNIT ( ) NAMED_UNIT ( * ) SI_UNIT ( .MILLI., .METRE. ) );
#4685 = EDGE_LOOP ( 'NONE', ( #1090, #6014, #8148, #2442 ) ) ;
#4686 = CARTESIAN_POINT ( 'NONE',  ( -2.862020680886494528, -76.20452850542926626, 4.100960146804039752 ) ) ;
#4687 = CARTESIAN_POINT ( 'NONE',  ( 43.45299461620743386, -9.999999999999994671, -1.500000000000000666 ) ) ;
#4688 = AXIS2_PLACEMENT_3D ( 'NONE', #1137, #1053, #4929 ) ;
#4689 = VECTOR ( 'NONE', #1106, 1000.000000000000000 ) ;
#4690 = PRODUCT_DEFINITION_FORMATION_WITH_SPECIFIED_SOURCE ( 'ANY', '', #2525, .NOT_KNOWN. ) ;
#4691 = CARTESIAN_POINT ( 'NONE',  ( 1.529537955723795140, -72.64547149457075648, 5.030887037049945221 ) ) ;
#4692 = CARTESIAN_POINT ( 'NONE',  ( -80.00000000000000000, -19.99999999999999645, -12.50000000000000355 ) ) ;
#4693 = CARTESIAN_POINT ( 'NONE',  ( -0.09506052544073276267, -96.49547149457075079, 4.999999999999997335 ) ) ;
#4694 = CARTESIAN_POINT ( 'NONE',  ( -4.037591185471424815, -61.20452850542925916, 5.718994135553947977 ) ) ;
#4695 = CARTESIAN_POINT ( 'NONE',  ( 75.00000000000000000, -9.999999999999994671, -1.500000000000000666 ) ) ;
#4696 = EDGE_CURVE ( 'NONE', #72, #1800, #2665, .T. ) ;
#4697 = FILL_AREA_STYLE ('',( #6724 ) ) ;
#4698 = CARTESIAN_POINT ( 'NONE',  ( 4.312004677471076519, -82.95452850542925205, 3.009306630940844496 ) ) ;
#4699 = CARTESIAN_POINT ( 'NONE',  ( 6.013306294175168709, -70.95452850542925205, 4.245374608440616093 ) ) ;
#4700 = ADVANCED_FACE ( 'NONE', ( #1271 ), #1310, .T. ) ;
#4701 = AXIS2_PLACEMENT_3D ( 'NONE', #4564, #4605, #737 ) ;
#4702 = CARTESIAN_POINT ( 'NONE',  ( -0.09506052544075634103, -78.49547149457075079, 2.999999999999997780 ) ) ;
#4703 = ORIENTED_EDGE ( 'NONE', *, *, #5322, .T. ) ;
#4704 = PLANE ( 'NONE',  #1529 ) ;
#4705 = DIRECTION ( 'NONE',  ( 1.000000000000000000, 0.000000000000000000, 0.000000000000000000 ) ) ;
#4706 = CARTESIAN_POINT ( 'NONE',  ( -5.257311121191323267, -81.75452850542926342, 0.09995255151729526277 ) ) ;
#4707 = VERTEX_POINT ( 'NONE', #3840 ) ;
#4708 = CARTESIAN_POINT ( 'NONE',  ( 1.529537955723689446, -68.85452850542924352, -5.030887037049978971 ) ) ;
#4709 = CARTESIAN_POINT ( 'NONE',  ( -2.610703060766924821, -87.04547149457074795, 1.773238653441125745 ) ) ;
#4710 = CARTESIAN_POINT ( 'NONE',  ( -0.8796985632579451542, -59.14547149457074227, -3.030887037049952326 ) ) ;
#4711 = CARTESIAN_POINT ( 'NONE',  ( -7.360235569667856304, -93.75452850542926342, 0.09995255151731782806 ) ) ;
#4712 = CARTESIAN_POINT ( 'NONE',  ( -2.823794231030022139, -69.90452850542925489, 1.017458915287783316 ) ) ;
#4713 = ORIENTED_EDGE ( 'NONE', *, *, #6386, .T. ) ;
#4714 = CARTESIAN_POINT ( 'NONE',  ( 50.00000000000000000, -20.00000000000000355, 7.499999999999996447 ) ) ;
#4715 = DIRECTION ( 'NONE',  ( -0.000000000000000000, 0.000000000000000000, 1.000000000000000000 ) ) ;
#4716 = CARTESIAN_POINT ( 'NONE',  ( 1.840261337453270585, -73.80452850542926058, 2.371175808195547852 ) ) ;
#4717 = CARTESIAN_POINT ( 'NONE',  ( -6.628020296210619833, -90.90452850542926910, 2.253526892787613978 ) ) ;
#4718 = CARTESIAN_POINT ( 'NONE',  ( 6.013306294175080779, -85.54547149457074795, -4.245374608440741326 ) ) ;
#4719 = CARTESIAN_POINT ( 'NONE',  ( 43.50000000000000711, -14.99999999999999467, 4.500000000000000888 ) ) ;
#4720 = LINE ( 'NONE', #4678, #2995 ) ;
#4721 = CARTESIAN_POINT ( 'NONE',  ( 1.069819614139493558, -70.84547149457073090, -2.969112962950042789 ) ) ;
#4722 = EDGE_CURVE ( 'NONE', #5453, #238, #6410, .T. ) ;
#4723 = CARTESIAN_POINT ( 'NONE',  ( 45.00000000000000000, -14.99999999999999467, 4.500000000000000888 ) ) ;
#4724 = ORIENTED_EDGE ( 'NONE', *, *, #6060, .T. ) ;
#4725 = CARTESIAN_POINT ( 'NONE',  ( 0.09506052544085895339, -67.50452850542926342, 4.999999999999997335 ) ) ;
#4726 = CARTESIAN_POINT ( 'NONE',  ( -4.191402346623057440, -81.19547149457073942, 5.607243785695398941 ) ) ;
#4727 =( NAMED_UNIT ( * ) PLANE_ANGLE_UNIT ( ) SI_UNIT ( $, .RADIAN. ) );
#4728 = ORIENTED_EDGE ( 'NONE', *, *, #6341, .T. ) ;
#4729 = CARTESIAN_POINT ( 'NONE',  ( -1.529537955723671683, -67.35452850542925773, 5.030887037049979860 ) ) ;
#4730 = DIRECTION ( 'NONE',  ( 0.000000000000000000, 0.000000000000000000, 1.000000000000000000 ) ) ;
#4731 = PRODUCT_RELATED_PRODUCT_CATEGORY ( 'part', '', ( #4875 ) ) ;
#4732 = CARTESIAN_POINT ( 'NONE',  ( 4.725907263620372056, -70.09547149457074511, 1.635492904037598283 ) ) ;
#4733 = CARTESIAN_POINT ( 'NONE',  ( -47.50000000000000711, -49.99999999999998579, 12.49999999999998224 ) ) ;
#4734 = CARTESIAN_POINT ( 'NONE',  ( -2.823794231030042123, -62.59547149457074511, -1.017458915287723364 ) ) ;
#4735 = CARTESIAN_POINT ( 'NONE',  ( 0.09506052544087911782, -58.50452850542925631, 6.999999999999997335 ) ) ;
#4736 = ORIENTED_EDGE ( 'NONE', *, *, #3178, .F. ) ;
#4737 = VECTOR ( 'NONE', #7644, 1000.000000000000000 ) ;
#4738 = SURFACE_STYLE_USAGE ( .BOTH. , #955 ) ;
#4739 = CARTESIAN_POINT ( 'NONE',  ( -1.719659006605370744, -90.15452850542922647, -4.969112962950016588 ) ) ;
#4740 = CARTESIAN_POINT ( 'NONE',  ( 1.069819614139494002, -73.84547149457073090, -2.969112962950042789 ) ) ;
#4741 = ORIENTED_EDGE ( 'NONE', *, *, #2795, .T. ) ;
#4742 = DIRECTION ( 'NONE',  ( 1.000000000000000000, 0.000000000000000000, 0.000000000000000000 ) ) ;
#4743 = CARTESIAN_POINT ( 'NONE',  ( 3.015831842038233734, -76.80452850542926058, 3.989209796945429432 ) ) ;
#4744 = ORIENTED_EDGE ( 'NONE', *, *, #3884, .T. ) ;
#4745 = CARTESIAN_POINT ( 'NONE',  ( -4.784657899331191011, -69.60452850542925773, -1.454677039711773867 ) ) ;
#4746 = CARTESIAN_POINT ( 'NONE',  ( 3.154386672714811102, -91.24547149457073658, 0.09995255151720662534 ) ) ;
#4747 = CARTESIAN_POINT ( 'NONE',  ( -2.882544866740859746, -59.89547149457074937, 0.8366430509619596778 ) ) ;
#4748 = CARTESIAN_POINT ( 'NONE',  ( -1.529537955723670350, -76.35452850542925773, 5.030887037049979860 ) ) ;
#4749 = CARTESIAN_POINT ( 'NONE',  ( -7.360235569667856304, -90.75452850542924921, 0.09995255151731782806 ) ) ;
#4750 = EDGE_CURVE ( 'NONE', #5131, #6672, #3085, .T. ) ;
#4751 = AXIS2_PLACEMENT_3D ( 'NONE', #4220, #4771, #6120 ) ;
#4752 = CARTESIAN_POINT ( 'NONE',  ( -2.610703060766966566, -66.45452850542925205, -1.773238653441072232 ) ) ;
#4754 = ADVANCED_FACE ( 'NONE', ( #673 ), #7126, .T. ) ;
#4753 = ORIENTED_EDGE ( 'NONE', *, *, #1919, .T. ) ;
#4755 = DIRECTION ( 'NONE',  ( -0.000000000000000000, -0.000000000000000000, -1.000000000000000000 ) ) ;
#4756 = AXIS2_PLACEMENT_3D ( 'NONE', #7910, #3982, #5917 ) ;
#4757 = DIRECTION ( 'NONE',  ( -1.051676107310939774E-14, -1.326812532709957139E-30, -1.000000000000000000 ) ) ;
#4758 = CARTESIAN_POINT ( 'NONE',  ( 2.882544866740897049, -77.10452850542924352, 0.8366430509618999478 ) ) ;
#4759 = VECTOR ( 'NONE', #217, 1000.000000000000114 ) ;
#4760 = CARTESIAN_POINT ( 'NONE',  ( 4.037591185471445243, -92.70452850542926626, -5.718994135553947977 ) ) ;
#4761 = AXIS2_PLACEMENT_3D ( 'NONE', #4812, #7389, #5488 ) ;
#4762 = CARTESIAN_POINT ( 'NONE',  ( 5.895805022753496161, -78.94547149457073942, 4.407101234057782868 ) ) ;
#4763 = CARTESIAN_POINT ( 'NONE',  ( -1.499999999999999556, -9.999999999999994671, -34.24264068711928388 ) ) ;
#4764 = CARTESIAN_POINT ( 'NONE',  ( 75.00000000000000000, -9.999999999999994671, -1.500000000000000666 ) ) ;
#4765 = CARTESIAN_POINT ( 'NONE',  ( 2.823794231030058111, -64.09547149457071669, 1.017458915287723809 ) ) ;
#4766 = CIRCLE ( 'NONE', #2223, 0.9999999999999948930 ) ;
#4767 = EDGE_CURVE ( 'NONE', #1450, #2779, #4459, .T. ) ;
#4768 = PRODUCT_DEFINITION_CONTEXT ( 'detailed design', #6632, 'design' ) ;
#4769 = FILL_AREA_STYLE ('',( #6159 ) ) ;
#4770 = ORIENTED_EDGE ( 'NONE', *, *, #3043, .T. ) ;
#4771 = DIRECTION ( 'NONE',  ( 0.2576626505603332173, -0.9662349396012460678, 0.000000000000000000 ) ) ;
#4772 = CARTESIAN_POINT ( 'NONE',  ( -1.529537955723671239, -70.35452850542925773, 5.030887037049979860 ) ) ;
#4773 = CARTESIAN_POINT ( 'NONE',  ( 2.369498399071078065, -79.84547149457074511, -6.969112962950057444 ) ) ;
#4774 = SURFACE_SIDE_STYLE ('',( #5406 ) ) ;
#4775 = ORIENTED_EDGE ( 'NONE', *, *, #3828, .T. ) ;
#4776 = CARTESIAN_POINT ( 'NONE',  ( -2.862020680886580681, -74.29547149457074795, -4.100960146803977580 ) ) ;
#4777 = CARTESIAN_POINT ( 'NONE',  ( 3.015831842038232402, -64.80452850542926058, 3.989209796945429432 ) ) ;
#4778 = FACE_OUTER_BOUND ( 'NONE', #4183, .T. ) ;
#4779 =( BOUNDED_SURFACE ( )  B_SPLINE_SURFACE ( 3, 2, ( 
 ( #1697, #3037, #7067, #4295, #614, #3908, #697, #5750, #6238, #6867, #3629, #1097, #4332, #7469, #4254, #8143, #2605, #4934, #8332, #5561, #6908, #3669, #6824, #2372, #7547, #1144, #6283, #7702, #1978, #1295, #5794, #3865, #22, #4529, #6195, #5524, #8104, #7155, #1547, #4739, #2735, #3948, #7835, #4570, #5840, #5295, #3368, #829, #110, #3447, #3991, #4611, #2021, #6601, #68, #5377, #7879, #2062, #1378, #3408, #5252, #6519, #3323, #2651, #1504, #6559, #7789, #5971, #6682, #872, #743, #2104, #5881, #5208, #2694, #7198, #5335, #2776, #1423, #7918, #4657, #197, #2144, #4072, #5928, #786, #6011, #4698, #3280, #235, #155, #7239, #1462, #4034, #7278, #6642, #2814, #7960, #2185, #7319, #4113, #279, #2857, #5420, #6054, #913, #3484, #5958, #7185, #4601, #144, #5153, #3981, #3400, #7866, #3353, #5782, #820, #3897, #2007, #2681, #185, #1452, #2725, #7268, #5283, #2094, #3225, #3312, #7735, #3937, #732, #4686, #4648, #5868, #5239, #6549, #1495, #99, #10, #4559, #1967, #2767, #1368, #7097, #4021, #686, #4517, #1323, #6505, #7230, #7778, #775, #4063, #642, #5916, #7823, #5198, #6466, #7143, #2052, #2590, #3267, #5823, #5328, #57, #6593, #2641, #1411, #7909, #2135, #4105, #6716, #2849, #905, #6673, #6167, #351, #1666, #8075, #269, #4867, #7951, #2305, #7309, #2176, #4910, #8116, #6086, #1535, #5410, #4729, #859, #311, #947, #4186, #3476, #6799, #7353, #7990, #5366, #1626, #3439, #392, #2889, #2219, #6043, #6757, #4777, #1580, #4146, #6002, #7438, #3518, #2806, #228, #5456, #8035, #2262, #4818, #7397, #2969, #2929, #4229, #1030, #989, #3599, #3557, #5534, #6126, #5494, #7481, #2341, #1709, #6630, #475, #5573, #6838, #6295, #4346, #1836, #1110, #4424, #4985, #5613, #3007, #7601, #1070, #6376, #3725, #3051, #8155, #4387, #6254, #2384, #4307, #3644, #2503, #7559, #433, #6963 ),
 ( #6338, #3766, #8192, #556, #513, #1195, #3134, #5064, #6923, #4944, #1876, #1235, #2463, #8232, #5689, #7518, #8273, #7008, #7643, #3806, #6209, #597, #1749, #2422, #3092, #3176, #5731, #8312, #2542, #5106, #7684, #6879, #1157, #3682, #1791, #5652, #4265, #5024, #2332, #6240, #1655, #341, #3631, #6788, #2294, #1780, #1146, #6115, #4936, #4215, #5563, #1615, #6910, #4256, #8145, #4897, #1021, #7509, #2374, #465, #3588, #1739, #6077, #2252, #4177, #4807, #6869, #4297, #3040, #8106, #6198, #6748, #4336, #1100, #4855, #3545, #423, #2411, #2959, #2918, #7549, #3672, #6826, #5602, #8183, #7429, #4974, #6156, #978, #2997, #1059, #301, #7471, #5484, #2878, #5445, #8025, #381, #7383, #5526, #8063, #1700, #8263, #8302, #6952, #5680, #2452, #8223, #4503, #503, #4457, #4377, #1228, #3124, #2534, #3880, #3081, #7039, #5723, #7589, #5183, #5096, #2023, #7125, #5056, #3715, #5644, #5014, #6369, #626, #7676, #1993, #1908, #6450, #7632, #6328, #1268, #4415, #2495, #7762, #6285, #3755, #2576, #1867, #3209, #1825, #4542, #3839, #5765, #6409, #6997, #5137, #7716, #671, #3798, #1952, #1186, #547, #588, #3168, #7082, #1308, #3252, #5808, #37, #2623, #5392, #4670, #5854, #82, #6657, #756, #7213, #7932, #4712, #886, #3384, #3460, #127, #6024, #6534, #7892, #249, #2664, #2749, #1479, #5941, #1437, #2830, #5223, #1391, #711, #7973, #4004, #7804, #2198, #7251, #4752, #209, #3298, #4047, #7290, #2118, #3422, #1352, #2708, #2788, #5895, #2037, #6615, #841, #3923, #169, #4585, #6490, #7168, #3964, #6574, #2159, #5268, #5986, #3337, #7849, #5310, #2075, #4628, #803, #5348, #1517, #4085, #8095, #8015, #4842, #6737, #6144, #7499, #6694, #2321, #1010, #2868, #454, #3577, #3619, #2402, #331, #7334, #924, #4125, #1644, #4247, #370, #5591, #2946, #1730, #2909, #1600, #4885, #8054, #3536, #3028, #1560 ),
 ( #5514, #2280, #6187, #413, #4285, #5474, #2986, #8172, #3496, #5434, #6067, #8134, #5553, #6859, #7459, #1688, #2241, #292, #6817, #4797, #7372, #1089, #967, #7420, #2364, #4927, #3660, #1050, #6229, #6105, #4166, #4204, #6777, #3867, #1134, #6358, #5084, #1218, #5046, #7069, #6274, #5003, #4324, #4491, #7620, #3069, #1297, #8292, #5796, #3827, #6897, #2520, #4447, #3743, #2441, #7664, #6436, #1854, #1814, #656, #3704, #5752, #1769, #5711, #5631, #2484, #4367, #3787, #5127, #492, #1898, #6985, #8212, #3239, #575, #1255, #24, #6315, #4961, #7575, #6941, #4404, #7027, #3157, #7539, #6398, #7704, #536, #1175, #616, #5669, #3114, #8251, #3197, #8334, #2566, #1937, #2106, #6479, #3449, #788, #4659, #7201, #3326, #1465, #7241, #5337, #745, #6604, #6013, #7112, #699, #1340, #3410, #4037, #2778, #4613, #2737, #3282, #6644, #5930, #3911, #5843, #7920, #2024, #112, #831, #5973, #2147, #1425, #4702, #1380, #7280, #7791, #3371, #1506, #71, #3993, #5297, #6562, #2697, #4074, #2653, #5210, #1980, #874, #5255, #4573, #2607, #157, #5170, #199, #4531, #7882, #7748, #3950, #7157, #6522, #5883, #7837, #2064, #4740, #2187, #7962, #237, #2816, #5381, #7301, #4640, #3975, #5996, #3432, #1569, #4679, #766, #7982, #4135, #5234, #5952, #895, #7222, #4721, #4596, #1446, #7260, #3347, #2085, #7179, #4014, #1404, #218, #7817, #2209, #7903, #6584, #6544, #2800, #814, #5906, #138, #2677, #6666, #3394, #2719, #5359, #3508, #6035, #5277, #1488, #7859, #2048, #178, #2761, #2168, #7942, #5320, #1528, #2127, #4098, #3469, #260, #4056, #6624, #2841, #5401, #851, #4765, #7345, #6703, #936, #93, #6690, #964, #921, #6141, #1515, #5471, #4162, #6021, #3616, #6734, #6771, #5550, #3493, #2156, #4082, #7288, #4794, #7417, #3532, #410, #6100, #2318, #6064, #4747, #8050, #2865, #288, #6184, #4710, #2195 ),
 ( #5428, #1007, #3573, #4882, #8011, #366, #2983, #6655, #245, #884, #2943, #5510, #7454, #327, #2277, #2826, #3457, #4838, #5389, #7970, #1684, #1557, #2238, #8092, #4244, #6813, #2906, #1046, #7368, #7331, #4122, #1641, #1597, #4201, #1172, #8247, #4364, #8208, #1894, #1086, #8169, #7495, #7661, #2438, #6226, #4444, #3111, #5000, #4282, #5708, #5081, #6311, #3740, #7616, #6855, #5666, #2517, #5628, #3784, #6938, #1851, #3025, #1127, #1809, #7024, #572, #4401, #6395, #6980, #1214, #2361, #7572, #3657, #3066, #532, #3823, #6354, #3152, #8288, #2480, #1251, #5043, #4923, #3701, #448, #612, #489, #5588, #3193, #2398, #4958, #7535, #8131, #1724, #6894, #1766, #4321, #6271, #3321, #6475, #1976, #1293, #1334, #4568, #2562, #7700, #20, #2734, #5165, #108, #5792, #7153, #4527, #5123, #3235, #5838, #7108, #2602, #7744, #5292, #7833, #785, #7196, #3906, #3989, #7065, #1420, #6432, #3863, #4145, #7237, #5206, #651, #695, #3278, #8330, #7787, #66, #5878, #2649, #5926, #2018, #1376, #4485, #741, #1932, #7877, #3946, #6517, #2693, #5250, #2061, #4609, #6557, #3366, #152, #2103, #4656, #1579, #946, #6715, #5748, #2340, #8034, #310, #1625, #6125, #5571, #3006, #4866, #8154, #2968, #6208, #432, #4306, #350, #474, #2928, #2383, #3555, #4908, #8074, #2887, #988, #3598, #2304, #5493, #7437, #3050, #4943, #6878, #7517, #1665, #1748, #4817, #1109, #4185, #7395, #1790, #4984, #5533, #6756, #4227, #6798, #6085, #8115, #6166, #1069, #1029, #3681, #391, #7480, #2261, #6837, #5455, #5612, #1708, #4264, #3643, #6252, #8191, #2421, #7558, #4345, #6921, #3517, #5651, #7047, #4550, #7089, #8231, #8311, #2462, #6294, #7599, #3765, #3217, #633, #2502, #5774, #596, #3846, #6415, #1960, #1234, #5023, #1316, #6459, #7683, #5105, #4, #1835, #4468, #3888, #7007, #5146, #2541, #2583, #4386, #5063, #3175 ),
 ( #6962, #4423, #3805, #5191, #7725, #4510, #680, #1277, #2632, #6375, #3724, #7642, #1194, #3260, #1875, #6337, #5816, #555, #3133, #5688, #5730, #46, #8271, #7769, #2000, #1156, #512, #1916, #3091, #2674, #2716, #5949, #3930, #721, #7939, #5992, #7298, #811, #7257, #5231, #2837, #2123, #3305, #5861, #4095, #6541, #4637, #5355, #2165, #6663, #3391, #892, #5903, #3466, #3972, #5317, #6032, #90, #175, #1485, #2757, #7219, #256, #7813, #7175, #6498, #5398, #1443, #2045, #7979, #4676, #2205, #215, #4593, #4053, #6621, #134, #1401, #848, #7134, #4011, #763, #1361, #4718, #7900, #3429, #3344, #5274, #2796, #7855, #2082, #1525, #6581, #6237, #1017, #5441, #4294, #462, #1566, #2290, #5560, #3542, #1056, #933, #975, #3585, #8022, #6744, #3504, #6074, #8142, #4132, #5523, #2249, #6112, #6152, #338, #420, #6700, #8103, #6785, #298, #3036, #378, #3628, #8180, #2915, #4762, #2875, #4804, #7426, #1696, #2955, #5599, #2329, #4933, #5481, #7380, #4893, #8060, #4851, #7341, #1611, #4173, #6194, #1652, #4253, #4212, #7468, #6823, #2993, #2371, #7506, #1736, #6866, #1096, #3668, #6407, #3250, #6907, #6282, #1143, #1226, #1906, #5642, #3752, #4412, #7714, #3207, #4455, #668, #7037, #1266, #4971, #5054, #3712, #5678, #2493, #6446, #624, #3837, #5761, #2531, #3878, #7629, #7546, #6326, #501, #5135, #3122, #3078, #2686, #2450, #8221, #5012, #8261, #2574, #1184, #5721, #5806, #2409, #8300, #1865, #6950, #7586, #545, #3796, #1777, #4331, #1823, #1950, #4375, #5093, #6995, #6367, #586, #3166, #7674, #4501, #7080, #1306, #81, #7931, #2116, #3420, #1477, #2036, #6614, #1350, #4046, #710, #3921, #6656, #1516, #7848, #3297, #4584, #6489, #2621, #2074, #125, #5940, #5222, #208, #755, #1390, #7122, #3383, #5180, #2158, #4627, #7167, #5853, #168, #3962, #2663, #7802, #7760, #840, #3336, #4540 ),
 ( #6533, #4669, #7891, #5894, #7250, #7211, #2747, #5309, #5985, #2707, #5267, #2787, #5346, #6573, #4003, #4711, #1436, #7289, #4083, #801, #885, #3459, #35, #1991, #7498, #2829, #3534, #6816, #4796, #2320, #2197, #2240, #2279, #923, #8013, #4749, #7333, #1048, #5391, #6773, #6692, #7370, #4841, #1599, #1686, #7972, #1009, #8052, #1559, #1727, #7419, #4884, #1088, #4165, #6023, #4124, #3495, #330, #2945, #1643, #4284, #4203, #6186, #6736, #290, #3576, #966, #6102, #6858, #247, #6066, #7456, #2908, #5513, #2867, #5431, #6143, #8094, #368, #5473, #4246, #3618, #412, #2985, #5552, #8133, #2363, #4925, #2401, #4446, #2519, #3825, #5668, #3786, #7538, #7703, #6982, #8171, #4960, #615, #3068, #1174, #1897, #7026, #3196, #8249, #5751, #2440, #8333, #491, #1853, #2565, #1768, #5045, #6357, #2482, #3742, #5126, #4323, #3703, #3027, #1936, #6313, #6896, #4489, #1217, #7068, #5083, #5590, #574, #3154, #5002, #1129, #5710, #3659, #535, #5630, #6228, #1254, #4403, #8291, #450, #7574, #7663, #8211, #6273, #6397, #1811, #4366, #6940, #3113, #7619, #2105, #6435, #2063, #1979, #5841, #111, #69, #5296, #654, #4612, #3324, #5168, #2777, #5882, #5929, #4699, #2652, #1296, #3238, #5795, #3949, #6560, #2695, #7919, #5254, #1463, #5209, #3910, #7199, #2022, #7790, #5336, #3866, #1337, #156, #4572, #787, #7747, #2145, #7836, #3369, #1424, #7156, #2736, #7880, #4035, #1379, #4658, #23, #2606, #4530, #7111, #7240, #6603, #830, #3992, #3409, #6478, #698, #5972, #3281, #6520, #198, #744, #873, #5378, #7961, #2186, #3448, #7279, #6012, #1505, #236, #2815, #4073, #6643, #8258, #6994, #3121, #6949, #623, #8179, #6904, #6235, #6406, #1183, #4970, #3205, #1864, #7713, #5720, #461, #4411, #6366, #5641, #4330, #1225, #5760, #3750, #3711, #2828, #4454, #7628, #584, #2573, #8220, #8299, #3077, #2408 ),
 ( #4374, #7673, #2449, #3165, #3035, #5010, #5677, #1775, #7583, #2530, #5598, #3795, #544, #7545, #5134, #2492, #5092, #1947, #1822, #6865, #1142, #3667, #6325, #1905, #5053, #1095, #7036, #1263, #3836, #6281, #500, #5221, #709, #207, #7930, #4539, #3382, #2662, #4002, #34, #5345, #2706, #6572, #754, #7801, #5939, #799, #7249, #2034, #166, #4500, #667, #2618, #3249, #5308, #2746, #4668, #6532, #4626, #5179, #2786, #7846, #5805, #7759, #1475, #3920, #4582, #7890, #2115, #4045, #3335, #6613, #3293, #839, #1349, #5265, #3419, #1990, #5893, #7210, #123, #7166, #5984, #7121, #6488, #3877, #7079, #1389, #5852, #1305, #2073, #6445, #80, #3961, #1435, #1360, #7812, #5190, #1558, #3304, #2631, #3929, #3887, #8012, #4592, #5815, #7332, #4839, #7369, #45, #246, #7768, #6458, #1999, #6497, #3494, #922, #2673, #6065, #762, #4123, #6691, #2239, #1400, #4549, #1598, #6735, #7971, #5390, #289, #7133, #4748, #4163, #7174, #5430, #5230, #720, #965, #2044, #5860, #4795, #89, #3971, #6540, #3458, #2866, #6022, #3533, #8051, #5472, #6101, #2827, #2196, #329, #2907, #2278, #679, #3259, #1315, #4365, #6815, #1767, #7455, #449, #3617, #6772, #4883, #7497, #6185, #1685, #4245, #6939, #1128, #2439, #490, #1047, #5629, #367, #3067, #8093, #2944, #5667, #533, #6856, #2319, #411, #5511, #1642, #1087, #1726, #4959, #2984, #7573, #8132, #5551, #6142, #2400, #7418, #8248, #2362, #4924, #4283, #7536, #3658, #6227, #3026, #4202, #8209, #5589, #3575, #4322, #2481, #5001, #8170, #6895, #3702, #1008, #6272, #1810, #1173, #3741, #6312, #3112, #4486, #7745, #1977, #5839, #5124, #1215, #2650, #2020, #3236, #652, #4528, #3785, #21, #7788, #2563, #696, #3864, #7109, #8290, #6396, #7066, #4569, #67, #1335, #3322, #3907, #6476, #7618, #7701, #6355, #8331, #1934, #742, #3279, #5207, #7154, #5166, #6518 ) ),
 .UNSPECIFIED., .T., .F., .T. ) 
 B_SPLINE_SURFACE_WITH_KNOTS ( ( 4, 3, 4 ),
 ( 3, 2, 2, 2, 2, 2, 2, 2, 2, 2, 2, 2, 2, 2, 2, 2, 2, 2, 2, 2, 2, 2, 2, 2, 2, 2, 2, 2, 2, 2, 2, 2, 2, 2, 2, 2, 2, 2, 2, 2, 2, 2, 2, 2, 2, 2, 2, 2, 2, 2, 2, 2, 2, 2, 2, 2, 2, 2, 2, 2, 2, 2, 2, 2, 2, 2, 2, 2, 2, 2, 2, 2, 2, 2, 2, 2, 2, 2, 2, 2, 2, 2, 2, 2, 2, 2, 2, 2, 2, 2, 2, 2, 2, 2, 2, 2, 2, 2, 2, 2, 2, 2, 2, 2, 2, 2, 2, 2, 2, 2, 2, 2, 2, 2, 2, 2, 2, 2, 2, 2, 2, 2, 2, 2, 2, 2, 2, 2, 2, 2, 3 ),
 ( 0.000000000000000000, 0.5000000000000000000, 1.000000000000000000 ),
 ( 0.000000000000000000, 0.007692307692307692735, 0.01538461538461538547, 0.02307692307692307820, 0.03076923076923077094, 0.03846153846153846367, 0.04615384615384615641, 0.05384615384615384914, 0.06153846153846154188, 0.06923076923076923461, 0.07692307692307692735, 0.08461538461538462008, 0.09230769230769231282, 0.1000000000000000056, 0.1076923076923076983, 0.1153846153846153910, 0.1230769230769230838, 0.1307692307692307765, 0.1384615384615384692, 0.1461538461538461620, 0.1538461538461538547, 0.1615384615384615474, 0.1692307692307692402, 0.1769230769230769329, 0.1846153846153846256, 0.1923076923076923184, 0.2000000000000000111, 0.2076923076923077038, 0.2153846153846153966, 0.2230769230769230893, 0.2307692307692307820, 0.2384615384615384748, 0.2461538461538461675, 0.2538461538461538325, 0.2615384615384615530, 0.2692307692307692180, 0.2769230769230769384, 0.2846153846153846034, 0.2923076923076923239, 0.2999999999999999889, 0.3076923076923077094, 0.3153846153846153744, 0.3230769230769230949, 0.3307692307692307598, 0.3384615384615384803, 0.3461538461538461453, 0.3538461538461538658, 0.3615384615384615308, 0.3692307692307692513, 0.3769230769230769162, 0.3846153846153846367, 0.3923076923076923017, 0.4000000000000000222, 0.4076923076923076872, 0.4153846153846154077, 0.4230769230769230727, 0.4307692307692307931, 0.4384615384615384581, 0.4461538461538461786, 0.4538461538461538436, 0.4615384615384615641, 0.4692307692307692291, 0.4769230769230769496, 0.4846153846153846145, 0.4923076923076923350, 0.5000000000000000000, 0.5076923076923076650, 0.5153846153846153300, 0.5230769230769231060, 0.5307692307692307709, 0.5384615384615384359, 0.5461538461538461009, 0.5538461538461538769, 0.5615384615384615419, 0.5692307692307692069, 0.5769230769230768718, 0.5846153846153846478, 0.5923076923076923128, 0.5999999999999999778, 0.6076923076923076428, 0.6153846153846154188, 0.6230769230769230838, 0.6307692307692307487, 0.6384615384615384137, 0.6461538461538461897, 0.6538461538461538547, 0.6615384615384615197, 0.6692307692307691847, 0.6769230769230769607, 0.6846153846153846256, 0.6923076923076922906, 0.6999999999999999556, 0.7076923076923077316, 0.7153846153846153966, 0.7230769230769230616, 0.7307692307692307265, 0.7384615384615385025, 0.7461538461538461675, 0.7538461538461538325, 0.7615384615384614975, 0.7692307692307692735, 0.7769230769230769384, 0.7846153846153846034, 0.7923076923076922684, 0.8000000000000000444, 0.8076923076923077094, 0.8153846153846153744, 0.8230769230769230393, 0.8307692307692308153, 0.8384615384615384803, 0.8461538461538461453, 0.8538461538461538103, 0.8615384615384615863, 0.8692307692307692513, 0.8769230769230769162, 0.8846153846153845812, 0.8923076923076923572, 0.9000000000000000222, 0.9076923076923076872, 0.9153846153846153522, 0.9230769230769231282, 0.9307692307692307931, 0.9384615384615384581, 0.9461538461538461231, 0.9538461538461538991, 0.9615384615384615641, 0.9692307692307692291, 0.9769230769230768940, 0.9846153846153846700, 0.9923076923076923350, 1.000000000000000000 ),
 .UNSPECIFIED. ) 
 GEOMETRIC_REPRESENTATION_ITEM ( )  RATIONAL_B_SPLINE_SURFACE ( (
 ( 1.000000000000000000, 0.9510565162951535312, 1.000000000000000000, 0.9510565162951535312, 1.000000000000000000, 0.9510565162951535312, 1.000000000000000000, 0.9510565162951535312, 1.000000000000000000, 0.9510565162951535312, 1.000000000000000000, 0.9510565162951535312, 1.000000000000000000, 0.9510565162951535312, 1.000000000000000000, 0.9510565162951535312, 1.000000000000000000, 0.9510565162951535312, 1.000000000000000000, 0.9510565162951535312, 1.000000000000000000, 0.9510565162951535312, 1.000000000000000000, 0.9510565162951535312, 1.000000000000000000, 0.9510565162951535312, 1.000000000000000000, 0.9510565162951535312, 1.000000000000000000, 0.9510565162951535312, 1.000000000000000000, 0.9510565162951535312, 1.000000000000000000, 0.9510565162951535312, 1.000000000000000000, 0.9510565162951535312, 1.000000000000000000, 0.9510565162951535312, 1.000000000000000000, 0.9510565162951535312, 1.000000000000000000, 0.9510565162951535312, 1.000000000000000000, 0.9510565162951535312, 1.000000000000000000, 0.9510565162951535312, 1.000000000000000000, 0.9510565162951535312, 1.000000000000000000, 0.9510565162951535312, 1.000000000000000000, 0.9510565162951535312, 1.000000000000000000, 0.9510565162951535312, 1.000000000000000000, 0.9510565162951535312, 1.000000000000000000, 0.9510565162951535312, 1.000000000000000000, 0.9510565162951535312, 1.000000000000000000, 0.9510565162951535312, 1.000000000000000000, 0.9510565162951535312, 1.000000000000000000, 0.9510565162951535312, 1.000000000000000000, 0.9510565162951535312, 1.000000000000000000, 0.9510565162951535312, 1.000000000000000000, 0.9510565162951535312, 1.000000000000000000, 0.9510565162951535312, 1.000000000000000000, 0.9510565162951535312, 1.000000000000000000, 0.9510565162951535312, 1.000000000000000000, 0.9510565162951535312, 1.000000000000000000, 0.9510565162951535312, 1.000000000000000000, 0.9510565162951535312, 1.000000000000000000, 0.9510565162951535312, 1.000000000000000000, 0.9510565162951535312, 1.000000000000000000, 0.9510565162951535312, 1.000000000000000000, 0.9510565162951535312, 1.000000000000000000, 0.9510565162951535312, 1.000000000000000000, 0.9510565162951535312, 1.000000000000000000, 0.9510565162951535312, 1.000000000000000000, 0.9510565162951535312, 1.000000000000000000, 0.9510565162951535312, 1.000000000000000000, 0.9510565162951535312, 1.000000000000000000, 0.9510565162951535312, 1.000000000000000000, 0.9510565162951535312, 1.000000000000000000, 0.9510565162951535312, 1.000000000000000000, 0.9510565162951535312, 1.000000000000000000, 0.9510565162951535312, 1.000000000000000000, 0.9510565162951535312, 1.000000000000000000, 0.9510565162951535312, 1.000000000000000000, 0.9510565162951535312, 1.000000000000000000, 0.9510565162951535312, 1.000000000000000000, 0.9510565162951535312, 1.000000000000000000, 0.9510565162951535312, 1.000000000000000000, 0.9510565162951535312, 1.000000000000000000, 0.9510565162951535312, 1.000000000000000000, 0.9510565162951535312, 1.000000000000000000, 0.9510565162951535312, 1.000000000000000000, 0.9510565162951535312, 1.000000000000000000, 0.9510565162951535312, 1.000000000000000000, 0.9510565162951535312, 1.000000000000000000, 0.9510565162951535312, 1.000000000000000000, 0.9510565162951535312, 1.000000000000000000, 0.9510565162951535312, 1.000000000000000000, 0.9510565162951535312, 1.000000000000000000, 0.9510565162951535312, 1.000000000000000000, 0.9510565162951535312, 1.000000000000000000, 0.9510565162951535312, 1.000000000000000000, 0.9510565162951535312, 1.000000000000000000, 0.9510565162951535312, 1.000000000000000000, 0.9510565162951535312, 1.000000000000000000, 0.9510565162951535312, 1.000000000000000000, 0.9510565162951535312, 1.000000000000000000, 0.9510565162951535312, 1.000000000000000000, 0.9510565162951535312, 1.000000000000000000, 0.9510565162951535312, 1.000000000000000000, 0.9510565162951535312, 1.000000000000000000, 0.9510565162951535312, 1.000000000000000000, 0.9510565162951535312, 1.000000000000000000, 0.9510565162951535312, 1.000000000000000000, 0.9510565162951535312, 1.000000000000000000, 0.9510565162951535312, 1.000000000000000000, 0.9510565162951535312, 1.000000000000000000, 0.9510565162951535312, 1.000000000000000000, 0.9510565162951535312, 1.000000000000000000, 0.9510565162951535312, 1.000000000000000000, 0.9510565162951535312, 1.000000000000000000, 0.9510565162951535312, 1.000000000000000000, 0.9510565162951535312, 1.000000000000000000, 0.9510565162951535312, 1.000000000000000000, 0.9510565162951535312, 1.000000000000000000, 0.9510565162951535312, 1.000000000000000000, 0.9510565162951535312, 1.000000000000000000, 0.9510565162951535312, 1.000000000000000000, 0.9510565162951535312, 1.000000000000000000, 0.9510565162951535312, 1.000000000000000000, 0.9510565162951535312, 1.000000000000000000, 0.9510565162951535312, 1.000000000000000000, 0.9510565162951535312, 1.000000000000000000, 0.9510565162951535312, 1.000000000000000000, 0.9510565162951535312, 1.000000000000000000, 0.9510565162951535312, 1.000000000000000000, 0.9510565162951535312, 1.000000000000000000, 0.9510565162951535312, 1.000000000000000000, 0.9510565162951535312, 1.000000000000000000, 0.9510565162951535312, 1.000000000000000000, 0.9510565162951535312, 1.000000000000000000, 0.9510565162951535312, 1.000000000000000000, 0.9510565162951535312, 1.000000000000000000, 0.9510565162951535312, 1.000000000000000000, 0.9510565162951535312, 1.000000000000000000, 0.9510565162951535312, 1.000000000000000000, 0.9510565162951535312, 1.000000000000000000, 0.9510565162951535312, 1.000000000000000000, 0.9510565162951535312, 1.000000000000000000, 0.9510565162951535312, 1.000000000000000000, 0.9510565162951535312, 1.000000000000000000, 0.9510565162951535312, 1.000000000000000000, 0.9510565162951535312, 1.000000000000000000, 0.9510565162951535312, 1.000000000000000000, 0.9510565162951535312, 1.000000000000000000),
 ( 0.3333333333333333703, 0.3170188387650512141, 0.3333333333333333703, 0.3170188387650512141, 0.3333333333333333703, 0.3170188387650512141, 0.3333333333333333703, 0.3170188387650512141, 0.3333333333333333703, 0.3170188387650512141, 0.3333333333333333703, 0.3170188387650512141, 0.3333333333333333703, 0.3170188387650512141, 0.3333333333333333703, 0.3170188387650512141, 0.3333333333333333703, 0.3170188387650512141, 0.3333333333333333703, 0.3170188387650512141, 0.3333333333333333703, 0.3170188387650512141, 0.3333333333333333703, 0.3170188387650512141, 0.3333333333333333703, 0.3170188387650512141, 0.3333333333333333703, 0.3170188387650512141, 0.3333333333333333703, 0.3170188387650512141, 0.3333333333333333703, 0.3170188387650512141, 0.3333333333333333703, 0.3170188387650512141, 0.3333333333333333703, 0.3170188387650512141, 0.3333333333333333703, 0.3170188387650512141, 0.3333333333333333703, 0.3170188387650512141, 0.3333333333333333703, 0.3170188387650512141, 0.3333333333333333703, 0.3170188387650512141, 0.3333333333333333703, 0.3170188387650512141, 0.3333333333333333703, 0.3170188387650512141, 0.3333333333333333703, 0.3170188387650512141, 0.3333333333333333703, 0.3170188387650512141, 0.3333333333333333703, 0.3170188387650512141, 0.3333333333333333703, 0.3170188387650512141, 0.3333333333333333703, 0.3170188387650512141, 0.3333333333333333703, 0.3170188387650512141, 0.3333333333333333703, 0.3170188387650512141, 0.3333333333333333703, 0.3170188387650512141, 0.3333333333333333703, 0.3170188387650512141, 0.3333333333333333703, 0.3170188387650512141, 0.3333333333333333703, 0.3170188387650512141, 0.3333333333333333703, 0.3170188387650512141, 0.3333333333333333703, 0.3170188387650512141, 0.3333333333333333703, 0.3170188387650512141, 0.3333333333333333703, 0.3170188387650512141, 0.3333333333333333703, 0.3170188387650512141, 0.3333333333333333703, 0.3170188387650512141, 0.3333333333333333703, 0.3170188387650512141, 0.3333333333333333703, 0.3170188387650512141, 0.3333333333333333703, 0.3170188387650512141, 0.3333333333333333703, 0.3170188387650512141, 0.3333333333333333703, 0.3170188387650512141, 0.3333333333333333703, 0.3170188387650512141, 0.3333333333333333703, 0.3170188387650512141, 0.3333333333333333703, 0.3170188387650512141, 0.3333333333333333703, 0.3170188387650512141, 0.3333333333333333703, 0.3170188387650512141, 0.3333333333333333703, 0.3170188387650512141, 0.3333333333333333703, 0.3170188387650512141, 0.3333333333333333703, 0.3170188387650512141, 0.3333333333333333703, 0.3170188387650512141, 0.3333333333333333703, 0.3170188387650512141, 0.3333333333333333703, 0.3170188387650512141, 0.3333333333333333703, 0.3170188387650512141, 0.3333333333333333703, 0.3170188387650512141, 0.3333333333333333703, 0.3170188387650512141, 0.3333333333333333703, 0.3170188387650512141, 0.3333333333333333703, 0.3170188387650512141, 0.3333333333333333703, 0.3170188387650512141, 0.3333333333333333703, 0.3170188387650512141, 0.3333333333333333703, 0.3170188387650512141, 0.3333333333333333703, 0.3170188387650512141, 0.3333333333333333703, 0.3170188387650512141, 0.3333333333333333703, 0.3170188387650512141, 0.3333333333333333703, 0.3170188387650512141, 0.3333333333333333703, 0.3170188387650512141, 0.3333333333333333703, 0.3170188387650512141, 0.3333333333333333703, 0.3170188387650512141, 0.3333333333333333703, 0.3170188387650512141, 0.3333333333333333703, 0.3170188387650512141, 0.3333333333333333703, 0.3170188387650512141, 0.3333333333333333703, 0.3170188387650512141, 0.3333333333333333703, 0.3170188387650512141, 0.3333333333333333703, 0.3170188387650512141, 0.3333333333333333703, 0.3170188387650512141, 0.3333333333333333703, 0.3170188387650512141, 0.3333333333333333703, 0.3170188387650512141, 0.3333333333333333703, 0.3170188387650512141, 0.3333333333333333703, 0.3170188387650512141, 0.3333333333333333703, 0.3170188387650512141, 0.3333333333333333703, 0.3170188387650512141, 0.3333333333333333703, 0.3170188387650512141, 0.3333333333333333703, 0.3170188387650512141, 0.3333333333333333703, 0.3170188387650512141, 0.3333333333333333703, 0.3170188387650512141, 0.3333333333333333703, 0.3170188387650512141, 0.3333333333333333703, 0.3170188387650512141, 0.3333333333333333703, 0.3170188387650512141, 0.3333333333333333703, 0.3170188387650512141, 0.3333333333333333703, 0.3170188387650512141, 0.3333333333333333703, 0.3170188387650512141, 0.3333333333333333703, 0.3170188387650512141, 0.3333333333333333703, 0.3170188387650512141, 0.3333333333333333703, 0.3170188387650512141, 0.3333333333333333703, 0.3170188387650512141, 0.3333333333333333703, 0.3170188387650512141, 0.3333333333333333703, 0.3170188387650512141, 0.3333333333333333703, 0.3170188387650512141, 0.3333333333333333703, 0.3170188387650512141, 0.3333333333333333703, 0.3170188387650512141, 0.3333333333333333703, 0.3170188387650512141, 0.3333333333333333703, 0.3170188387650512141, 0.3333333333333333703, 0.3170188387650512141, 0.3333333333333333703, 0.3170188387650512141, 0.3333333333333333703, 0.3170188387650512141, 0.3333333333333333703, 0.3170188387650512141, 0.3333333333333333703, 0.3170188387650512141, 0.3333333333333333703, 0.3170188387650512141, 0.3333333333333333703, 0.3170188387650512141, 0.3333333333333333703, 0.3170188387650512141, 0.3333333333333333703, 0.3170188387650512141, 0.3333333333333333703, 0.3170188387650512141, 0.3333333333333333703, 0.3170188387650512141, 0.3333333333333333703, 0.3170188387650512141, 0.3333333333333333703, 0.3170188387650512141, 0.3333333333333333703, 0.3170188387650512141, 0.3333333333333333703, 0.3170188387650512141, 0.3333333333333333703, 0.3170188387650512141, 0.3333333333333333703, 0.3170188387650512141, 0.3333333333333333703, 0.3170188387650512141, 0.3333333333333333703, 0.3170188387650512141, 0.3333333333333333703, 0.3170188387650512141, 0.3333333333333333703, 0.3170188387650512141, 0.3333333333333333703, 0.3170188387650512141, 0.3333333333333333703, 0.3170188387650512141, 0.3333333333333333703, 0.3170188387650512141, 0.3333333333333333703),
 ( 0.3333333333333333703, 0.3170188387650512141, 0.3333333333333333703, 0.3170188387650512141, 0.3333333333333333703, 0.3170188387650512141, 0.3333333333333333703, 0.3170188387650512141, 0.3333333333333333703, 0.3170188387650512141, 0.3333333333333333703, 0.3170188387650512141, 0.3333333333333333703, 0.3170188387650512141, 0.3333333333333333703, 0.3170188387650512141, 0.3333333333333333703, 0.3170188387650512141, 0.3333333333333333703, 0.3170188387650512141, 0.3333333333333333703, 0.3170188387650512141, 0.3333333333333333703, 0.3170188387650512141, 0.3333333333333333703, 0.3170188387650512141, 0.3333333333333333703, 0.3170188387650512141, 0.3333333333333333703, 0.3170188387650512141, 0.3333333333333333703, 0.3170188387650512141, 0.3333333333333333703, 0.3170188387650512141, 0.3333333333333333703, 0.3170188387650512141, 0.3333333333333333703, 0.3170188387650512141, 0.3333333333333333703, 0.3170188387650512141, 0.3333333333333333703, 0.3170188387650512141, 0.3333333333333333703, 0.3170188387650512141, 0.3333333333333333703, 0.3170188387650512141, 0.3333333333333333703, 0.3170188387650512141, 0.3333333333333333703, 0.3170188387650512141, 0.3333333333333333703, 0.3170188387650512141, 0.3333333333333333703, 0.3170188387650512141, 0.3333333333333333703, 0.3170188387650512141, 0.3333333333333333703, 0.3170188387650512141, 0.3333333333333333703, 0.3170188387650512141, 0.3333333333333333703, 0.3170188387650512141, 0.3333333333333333703, 0.3170188387650512141, 0.3333333333333333703, 0.3170188387650512141, 0.3333333333333333703, 0.3170188387650512141, 0.3333333333333333703, 0.3170188387650512141, 0.3333333333333333703, 0.3170188387650512141, 0.3333333333333333703, 0.3170188387650512141, 0.3333333333333333703, 0.3170188387650512141, 0.3333333333333333703, 0.3170188387650512141, 0.3333333333333333703, 0.3170188387650512141, 0.3333333333333333703, 0.3170188387650512141, 0.3333333333333333703, 0.3170188387650512141, 0.3333333333333333703, 0.3170188387650512141, 0.3333333333333333703, 0.3170188387650512141, 0.3333333333333333703, 0.3170188387650512141, 0.3333333333333333703, 0.3170188387650512141, 0.3333333333333333703, 0.3170188387650512141, 0.3333333333333333703, 0.3170188387650512141, 0.3333333333333333703, 0.3170188387650512141, 0.3333333333333333703, 0.3170188387650512141, 0.3333333333333333703, 0.3170188387650512141, 0.3333333333333333703, 0.3170188387650512141, 0.3333333333333333703, 0.3170188387650512141, 0.3333333333333333703, 0.3170188387650512141, 0.3333333333333333703, 0.3170188387650512141, 0.3333333333333333703, 0.3170188387650512141, 0.3333333333333333703, 0.3170188387650512141, 0.3333333333333333703, 0.3170188387650512141, 0.3333333333333333703, 0.3170188387650512141, 0.3333333333333333703, 0.3170188387650512141, 0.3333333333333333703, 0.3170188387650512141, 0.3333333333333333703, 0.3170188387650512141, 0.3333333333333333703, 0.3170188387650512141, 0.3333333333333333703, 0.3170188387650512141, 0.3333333333333333703, 0.3170188387650512141, 0.3333333333333333703, 0.3170188387650512141, 0.3333333333333333703, 0.3170188387650512141, 0.3333333333333333703, 0.3170188387650512141, 0.3333333333333333703, 0.3170188387650512141, 0.3333333333333333703, 0.3170188387650512141, 0.3333333333333333703, 0.3170188387650512141, 0.3333333333333333703, 0.3170188387650512141, 0.3333333333333333703, 0.3170188387650512141, 0.3333333333333333703, 0.3170188387650512141, 0.3333333333333333703, 0.3170188387650512141, 0.3333333333333333703, 0.3170188387650512141, 0.3333333333333333703, 0.3170188387650512141, 0.3333333333333333703, 0.3170188387650512141, 0.3333333333333333703, 0.3170188387650512141, 0.3333333333333333703, 0.3170188387650512141, 0.3333333333333333703, 0.3170188387650512141, 0.3333333333333333703, 0.3170188387650512141, 0.3333333333333333703, 0.3170188387650512141, 0.3333333333333333703, 0.3170188387650512141, 0.3333333333333333703, 0.3170188387650512141, 0.3333333333333333703, 0.3170188387650512141, 0.3333333333333333703, 0.3170188387650512141, 0.3333333333333333703, 0.3170188387650512141, 0.3333333333333333703, 0.3170188387650512141, 0.3333333333333333703, 0.3170188387650512141, 0.3333333333333333703, 0.3170188387650512141, 0.3333333333333333703, 0.3170188387650512141, 0.3333333333333333703, 0.3170188387650512141, 0.3333333333333333703, 0.3170188387650512141, 0.3333333333333333703, 0.3170188387650512141, 0.3333333333333333703, 0.3170188387650512141, 0.3333333333333333703, 0.3170188387650512141, 0.3333333333333333703, 0.3170188387650512141, 0.3333333333333333703, 0.3170188387650512141, 0.3333333333333333703, 0.3170188387650512141, 0.3333333333333333703, 0.3170188387650512141, 0.3333333333333333703, 0.3170188387650512141, 0.3333333333333333703, 0.3170188387650512141, 0.3333333333333333703, 0.3170188387650512141, 0.3333333333333333703, 0.3170188387650512141, 0.3333333333333333703, 0.3170188387650512141, 0.3333333333333333703, 0.3170188387650512141, 0.3333333333333333703, 0.3170188387650512141, 0.3333333333333333703, 0.3170188387650512141, 0.3333333333333333703, 0.3170188387650512141, 0.3333333333333333703, 0.3170188387650512141, 0.3333333333333333703, 0.3170188387650512141, 0.3333333333333333703, 0.3170188387650512141, 0.3333333333333333703, 0.3170188387650512141, 0.3333333333333333703, 0.3170188387650512141, 0.3333333333333333703, 0.3170188387650512141, 0.3333333333333333703, 0.3170188387650512141, 0.3333333333333333703, 0.3170188387650512141, 0.3333333333333333703, 0.3170188387650512141, 0.3333333333333333703, 0.3170188387650512141, 0.3333333333333333703, 0.3170188387650512141, 0.3333333333333333703, 0.3170188387650512141, 0.3333333333333333703, 0.3170188387650512141, 0.3333333333333333703, 0.3170188387650512141, 0.3333333333333333703, 0.3170188387650512141, 0.3333333333333333703, 0.3170188387650512141, 0.3333333333333333703, 0.3170188387650512141, 0.3333333333333333703, 0.3170188387650512141, 0.3333333333333333703, 0.3170188387650512141, 0.3333333333333333703, 0.3170188387650512141, 0.3333333333333333703),
 ( 1.000000000000000000, 0.9510565162951535312, 1.000000000000000000, 0.9510565162951535312, 1.000000000000000000, 0.9510565162951535312, 1.000000000000000000, 0.9510565162951535312, 1.000000000000000000, 0.9510565162951535312, 1.000000000000000000, 0.9510565162951535312, 1.000000000000000000, 0.9510565162951535312, 1.000000000000000000, 0.9510565162951535312, 1.000000000000000000, 0.9510565162951535312, 1.000000000000000000, 0.9510565162951535312, 1.000000000000000000, 0.9510565162951535312, 1.000000000000000000, 0.9510565162951535312, 1.000000000000000000, 0.9510565162951535312, 1.000000000000000000, 0.9510565162951535312, 1.000000000000000000, 0.9510565162951535312, 1.000000000000000000, 0.9510565162951535312, 1.000000000000000000, 0.9510565162951535312, 1.000000000000000000, 0.9510565162951535312, 1.000000000000000000, 0.9510565162951535312, 1.000000000000000000, 0.9510565162951535312, 1.000000000000000000, 0.9510565162951535312, 1.000000000000000000, 0.9510565162951535312, 1.000000000000000000, 0.9510565162951535312, 1.000000000000000000, 0.9510565162951535312, 1.000000000000000000, 0.9510565162951535312, 1.000000000000000000, 0.9510565162951535312, 1.000000000000000000, 0.9510565162951535312, 1.000000000000000000, 0.9510565162951535312, 1.000000000000000000, 0.9510565162951535312, 1.000000000000000000, 0.9510565162951535312, 1.000000000000000000, 0.9510565162951535312, 1.000000000000000000, 0.9510565162951535312, 1.000000000000000000, 0.9510565162951535312, 1.000000000000000000, 0.9510565162951535312, 1.000000000000000000, 0.9510565162951535312, 1.000000000000000000, 0.9510565162951535312, 1.000000000000000000, 0.9510565162951535312, 1.000000000000000000, 0.9510565162951535312, 1.000000000000000000, 0.9510565162951535312, 1.000000000000000000, 0.9510565162951535312, 1.000000000000000000, 0.9510565162951535312, 1.000000000000000000, 0.9510565162951535312, 1.000000000000000000, 0.9510565162951535312, 1.000000000000000000, 0.9510565162951535312, 1.000000000000000000, 0.9510565162951535312, 1.000000000000000000, 0.9510565162951535312, 1.000000000000000000, 0.9510565162951535312, 1.000000000000000000, 0.9510565162951535312, 1.000000000000000000, 0.9510565162951535312, 1.000000000000000000, 0.9510565162951535312, 1.000000000000000000, 0.9510565162951535312, 1.000000000000000000, 0.9510565162951535312, 1.000000000000000000, 0.9510565162951535312, 1.000000000000000000, 0.9510565162951535312, 1.000000000000000000, 0.9510565162951535312, 1.000000000000000000, 0.9510565162951535312, 1.000000000000000000, 0.9510565162951535312, 1.000000000000000000, 0.9510565162951535312, 1.000000000000000000, 0.9510565162951535312, 1.000000000000000000, 0.9510565162951535312, 1.000000000000000000, 0.9510565162951535312, 1.000000000000000000, 0.9510565162951535312, 1.000000000000000000, 0.9510565162951535312, 1.000000000000000000, 0.9510565162951535312, 1.000000000000000000, 0.9510565162951535312, 1.000000000000000000, 0.9510565162951535312, 1.000000000000000000, 0.9510565162951535312, 1.000000000000000000, 0.9510565162951535312, 1.000000000000000000, 0.9510565162951535312, 1.000000000000000000, 0.9510565162951535312, 1.000000000000000000, 0.9510565162951535312, 1.000000000000000000, 0.9510565162951535312, 1.000000000000000000, 0.9510565162951535312, 1.000000000000000000, 0.9510565162951535312, 1.000000000000000000, 0.9510565162951535312, 1.000000000000000000, 0.9510565162951535312, 1.000000000000000000, 0.9510565162951535312, 1.000000000000000000, 0.9510565162951535312, 1.000000000000000000, 0.9510565162951535312, 1.000000000000000000, 0.9510565162951535312, 1.000000000000000000, 0.9510565162951535312, 1.000000000000000000, 0.9510565162951535312, 1.000000000000000000, 0.9510565162951535312, 1.000000000000000000, 0.9510565162951535312, 1.000000000000000000, 0.9510565162951535312, 1.000000000000000000, 0.9510565162951535312, 1.000000000000000000, 0.9510565162951535312, 1.000000000000000000, 0.9510565162951535312, 1.000000000000000000, 0.9510565162951535312, 1.000000000000000000, 0.9510565162951535312, 1.000000000000000000, 0.9510565162951535312, 1.000000000000000000, 0.9510565162951535312, 1.000000000000000000, 0.9510565162951535312, 1.000000000000000000, 0.9510565162951535312, 1.000000000000000000, 0.9510565162951535312, 1.000000000000000000, 0.9510565162951535312, 1.000000000000000000, 0.9510565162951535312, 1.000000000000000000, 0.9510565162951535312, 1.000000000000000000, 0.9510565162951535312, 1.000000000000000000, 0.9510565162951535312, 1.000000000000000000, 0.9510565162951535312, 1.000000000000000000, 0.9510565162951535312, 1.000000000000000000, 0.9510565162951535312, 1.000000000000000000, 0.9510565162951535312, 1.000000000000000000, 0.9510565162951535312, 1.000000000000000000, 0.9510565162951535312, 1.000000000000000000, 0.9510565162951535312, 1.000000000000000000, 0.9510565162951535312, 1.000000000000000000, 0.9510565162951535312, 1.000000000000000000, 0.9510565162951535312, 1.000000000000000000, 0.9510565162951535312, 1.000000000000000000, 0.9510565162951535312, 1.000000000000000000, 0.9510565162951535312, 1.000000000000000000, 0.9510565162951535312, 1.000000000000000000, 0.9510565162951535312, 1.000000000000000000, 0.9510565162951535312, 1.000000000000000000, 0.9510565162951535312, 1.000000000000000000, 0.9510565162951535312, 1.000000000000000000, 0.9510565162951535312, 1.000000000000000000, 0.9510565162951535312, 1.000000000000000000, 0.9510565162951535312, 1.000000000000000000, 0.9510565162951535312, 1.000000000000000000, 0.9510565162951535312, 1.000000000000000000, 0.9510565162951535312, 1.000000000000000000, 0.9510565162951535312, 1.000000000000000000, 0.9510565162951535312, 1.000000000000000000, 0.9510565162951535312, 1.000000000000000000, 0.9510565162951535312, 1.000000000000000000, 0.9510565162951535312, 1.000000000000000000, 0.9510565162951535312, 1.000000000000000000),
 ( 0.3333333333333333703, 0.3170188387650512141, 0.3333333333333333703, 0.3170188387650512141, 0.3333333333333333703, 0.3170188387650512141, 0.3333333333333333703, 0.3170188387650512141, 0.3333333333333333703, 0.3170188387650512141, 0.3333333333333333703, 0.3170188387650512141, 0.3333333333333333703, 0.3170188387650512141, 0.3333333333333333703, 0.3170188387650512141, 0.3333333333333333703, 0.3170188387650512141, 0.3333333333333333703, 0.3170188387650512141, 0.3333333333333333703, 0.3170188387650512141, 0.3333333333333333703, 0.3170188387650512141, 0.3333333333333333703, 0.3170188387650512141, 0.3333333333333333703, 0.3170188387650512141, 0.3333333333333333703, 0.3170188387650512141, 0.3333333333333333703, 0.3170188387650512141, 0.3333333333333333703, 0.3170188387650512141, 0.3333333333333333703, 0.3170188387650512141, 0.3333333333333333703, 0.3170188387650512141, 0.3333333333333333703, 0.3170188387650512141, 0.3333333333333333703, 0.3170188387650512141, 0.3333333333333333703, 0.3170188387650512141, 0.3333333333333333703, 0.3170188387650512141, 0.3333333333333333703, 0.3170188387650512141, 0.3333333333333333703, 0.3170188387650512141, 0.3333333333333333703, 0.3170188387650512141, 0.3333333333333333703, 0.3170188387650512141, 0.3333333333333333703, 0.3170188387650512141, 0.3333333333333333703, 0.3170188387650512141, 0.3333333333333333703, 0.3170188387650512141, 0.3333333333333333703, 0.3170188387650512141, 0.3333333333333333703, 0.3170188387650512141, 0.3333333333333333703, 0.3170188387650512141, 0.3333333333333333703, 0.3170188387650512141, 0.3333333333333333703, 0.3170188387650512141, 0.3333333333333333703, 0.3170188387650512141, 0.3333333333333333703, 0.3170188387650512141, 0.3333333333333333703, 0.3170188387650512141, 0.3333333333333333703, 0.3170188387650512141, 0.3333333333333333703, 0.3170188387650512141, 0.3333333333333333703, 0.3170188387650512141, 0.3333333333333333703, 0.3170188387650512141, 0.3333333333333333703, 0.3170188387650512141, 0.3333333333333333703, 0.3170188387650512141, 0.3333333333333333703, 0.3170188387650512141, 0.3333333333333333703, 0.3170188387650512141, 0.3333333333333333703, 0.3170188387650512141, 0.3333333333333333703, 0.3170188387650512141, 0.3333333333333333703, 0.3170188387650512141, 0.3333333333333333703, 0.3170188387650512141, 0.3333333333333333703, 0.3170188387650512141, 0.3333333333333333703, 0.3170188387650512141, 0.3333333333333333703, 0.3170188387650512141, 0.3333333333333333703, 0.3170188387650512141, 0.3333333333333333703, 0.3170188387650512141, 0.3333333333333333703, 0.3170188387650512141, 0.3333333333333333703, 0.3170188387650512141, 0.3333333333333333703, 0.3170188387650512141, 0.3333333333333333703, 0.3170188387650512141, 0.3333333333333333703, 0.3170188387650512141, 0.3333333333333333703, 0.3170188387650512141, 0.3333333333333333703, 0.3170188387650512141, 0.3333333333333333703, 0.3170188387650512141, 0.3333333333333333703, 0.3170188387650512141, 0.3333333333333333703, 0.3170188387650512141, 0.3333333333333333703, 0.3170188387650512141, 0.3333333333333333703, 0.3170188387650512141, 0.3333333333333333703, 0.3170188387650512141, 0.3333333333333333703, 0.3170188387650512141, 0.3333333333333333703, 0.3170188387650512141, 0.3333333333333333703, 0.3170188387650512141, 0.3333333333333333703, 0.3170188387650512141, 0.3333333333333333703, 0.3170188387650512141, 0.3333333333333333703, 0.3170188387650512141, 0.3333333333333333703, 0.3170188387650512141, 0.3333333333333333703, 0.3170188387650512141, 0.3333333333333333703, 0.3170188387650512141, 0.3333333333333333703, 0.3170188387650512141, 0.3333333333333333703, 0.3170188387650512141, 0.3333333333333333703, 0.3170188387650512141, 0.3333333333333333703, 0.3170188387650512141, 0.3333333333333333703, 0.3170188387650512141, 0.3333333333333333703, 0.3170188387650512141, 0.3333333333333333703, 0.3170188387650512141, 0.3333333333333333703, 0.3170188387650512141, 0.3333333333333333703, 0.3170188387650512141, 0.3333333333333333703, 0.3170188387650512141, 0.3333333333333333703, 0.3170188387650512141, 0.3333333333333333703, 0.3170188387650512141, 0.3333333333333333703, 0.3170188387650512141, 0.3333333333333333703, 0.3170188387650512141, 0.3333333333333333703, 0.3170188387650512141, 0.3333333333333333703, 0.3170188387650512141, 0.3333333333333333703, 0.3170188387650512141, 0.3333333333333333703, 0.3170188387650512141, 0.3333333333333333703, 0.3170188387650512141, 0.3333333333333333703, 0.3170188387650512141, 0.3333333333333333703, 0.3170188387650512141, 0.3333333333333333703, 0.3170188387650512141, 0.3333333333333333703, 0.3170188387650512141, 0.3333333333333333703, 0.3170188387650512141, 0.3333333333333333703, 0.3170188387650512141, 0.3333333333333333703, 0.3170188387650512141, 0.3333333333333333703, 0.3170188387650512141, 0.3333333333333333703, 0.3170188387650512141, 0.3333333333333333703, 0.3170188387650512141, 0.3333333333333333703, 0.3170188387650512141, 0.3333333333333333703, 0.3170188387650512141, 0.3333333333333333703, 0.3170188387650512141, 0.3333333333333333703, 0.3170188387650512141, 0.3333333333333333703, 0.3170188387650512141, 0.3333333333333333703, 0.3170188387650512141, 0.3333333333333333703, 0.3170188387650512141, 0.3333333333333333703, 0.3170188387650512141, 0.3333333333333333703, 0.3170188387650512141, 0.3333333333333333703, 0.3170188387650512141, 0.3333333333333333703, 0.3170188387650512141, 0.3333333333333333703, 0.3170188387650512141, 0.3333333333333333703, 0.3170188387650512141, 0.3333333333333333703, 0.3170188387650512141, 0.3333333333333333703, 0.3170188387650512141, 0.3333333333333333703, 0.3170188387650512141, 0.3333333333333333703, 0.3170188387650512141, 0.3333333333333333703, 0.3170188387650512141, 0.3333333333333333703, 0.3170188387650512141, 0.3333333333333333703, 0.3170188387650512141, 0.3333333333333333703, 0.3170188387650512141, 0.3333333333333333703, 0.3170188387650512141, 0.3333333333333333703, 0.3170188387650512141, 0.3333333333333333703, 0.3170188387650512141, 0.3333333333333333703),
 ( 0.3333333333333333703, 0.3170188387650512141, 0.3333333333333333703, 0.3170188387650512141, 0.3333333333333333703, 0.3170188387650512141, 0.3333333333333333703, 0.3170188387650512141, 0.3333333333333333703, 0.3170188387650512141, 0.3333333333333333703, 0.3170188387650512141, 0.3333333333333333703, 0.3170188387650512141, 0.3333333333333333703, 0.3170188387650512141, 0.3333333333333333703, 0.3170188387650512141, 0.3333333333333333703, 0.3170188387650512141, 0.3333333333333333703, 0.3170188387650512141, 0.3333333333333333703, 0.3170188387650512141, 0.3333333333333333703, 0.3170188387650512141, 0.3333333333333333703, 0.3170188387650512141, 0.3333333333333333703, 0.3170188387650512141, 0.3333333333333333703, 0.3170188387650512141, 0.3333333333333333703, 0.3170188387650512141, 0.3333333333333333703, 0.3170188387650512141, 0.3333333333333333703, 0.3170188387650512141, 0.3333333333333333703, 0.3170188387650512141, 0.3333333333333333703, 0.3170188387650512141, 0.3333333333333333703, 0.3170188387650512141, 0.3333333333333333703, 0.3170188387650512141, 0.3333333333333333703, 0.3170188387650512141, 0.3333333333333333703, 0.3170188387650512141, 0.3333333333333333703, 0.3170188387650512141, 0.3333333333333333703, 0.3170188387650512141, 0.3333333333333333703, 0.3170188387650512141, 0.3333333333333333703, 0.3170188387650512141, 0.3333333333333333703, 0.3170188387650512141, 0.3333333333333333703, 0.3170188387650512141, 0.3333333333333333703, 0.3170188387650512141, 0.3333333333333333703, 0.3170188387650512141, 0.3333333333333333703, 0.3170188387650512141, 0.3333333333333333703, 0.3170188387650512141, 0.3333333333333333703, 0.3170188387650512141, 0.3333333333333333703, 0.3170188387650512141, 0.3333333333333333703, 0.3170188387650512141, 0.3333333333333333703, 0.3170188387650512141, 0.3333333333333333703, 0.3170188387650512141, 0.3333333333333333703, 0.3170188387650512141, 0.3333333333333333703, 0.3170188387650512141, 0.3333333333333333703, 0.3170188387650512141, 0.3333333333333333703, 0.3170188387650512141, 0.3333333333333333703, 0.3170188387650512141, 0.3333333333333333703, 0.3170188387650512141, 0.3333333333333333703, 0.3170188387650512141, 0.3333333333333333703, 0.3170188387650512141, 0.3333333333333333703, 0.3170188387650512141, 0.3333333333333333703, 0.3170188387650512141, 0.3333333333333333703, 0.3170188387650512141, 0.3333333333333333703, 0.3170188387650512141, 0.3333333333333333703, 0.3170188387650512141, 0.3333333333333333703, 0.3170188387650512141, 0.3333333333333333703, 0.3170188387650512141, 0.3333333333333333703, 0.3170188387650512141, 0.3333333333333333703, 0.3170188387650512141, 0.3333333333333333703, 0.3170188387650512141, 0.3333333333333333703, 0.3170188387650512141, 0.3333333333333333703, 0.3170188387650512141, 0.3333333333333333703, 0.3170188387650512141, 0.3333333333333333703, 0.3170188387650512141, 0.3333333333333333703, 0.3170188387650512141, 0.3333333333333333703, 0.3170188387650512141, 0.3333333333333333703, 0.3170188387650512141, 0.3333333333333333703, 0.3170188387650512141, 0.3333333333333333703, 0.3170188387650512141, 0.3333333333333333703, 0.3170188387650512141, 0.3333333333333333703, 0.3170188387650512141, 0.3333333333333333703, 0.3170188387650512141, 0.3333333333333333703, 0.3170188387650512141, 0.3333333333333333703, 0.3170188387650512141, 0.3333333333333333703, 0.3170188387650512141, 0.3333333333333333703, 0.3170188387650512141, 0.3333333333333333703, 0.3170188387650512141, 0.3333333333333333703, 0.3170188387650512141, 0.3333333333333333703, 0.3170188387650512141, 0.3333333333333333703, 0.3170188387650512141, 0.3333333333333333703, 0.3170188387650512141, 0.3333333333333333703, 0.3170188387650512141, 0.3333333333333333703, 0.3170188387650512141, 0.3333333333333333703, 0.3170188387650512141, 0.3333333333333333703, 0.3170188387650512141, 0.3333333333333333703, 0.3170188387650512141, 0.3333333333333333703, 0.3170188387650512141, 0.3333333333333333703, 0.3170188387650512141, 0.3333333333333333703, 0.3170188387650512141, 0.3333333333333333703, 0.3170188387650512141, 0.3333333333333333703, 0.3170188387650512141, 0.3333333333333333703, 0.3170188387650512141, 0.3333333333333333703, 0.3170188387650512141, 0.3333333333333333703, 0.3170188387650512141, 0.3333333333333333703, 0.3170188387650512141, 0.3333333333333333703, 0.3170188387650512141, 0.3333333333333333703, 0.3170188387650512141, 0.3333333333333333703, 0.3170188387650512141, 0.3333333333333333703, 0.3170188387650512141, 0.3333333333333333703, 0.3170188387650512141, 0.3333333333333333703, 0.3170188387650512141, 0.3333333333333333703, 0.3170188387650512141, 0.3333333333333333703, 0.3170188387650512141, 0.3333333333333333703, 0.3170188387650512141, 0.3333333333333333703, 0.3170188387650512141, 0.3333333333333333703, 0.3170188387650512141, 0.3333333333333333703, 0.3170188387650512141, 0.3333333333333333703, 0.3170188387650512141, 0.3333333333333333703, 0.3170188387650512141, 0.3333333333333333703, 0.3170188387650512141, 0.3333333333333333703, 0.3170188387650512141, 0.3333333333333333703, 0.3170188387650512141, 0.3333333333333333703, 0.3170188387650512141, 0.3333333333333333703, 0.3170188387650512141, 0.3333333333333333703, 0.3170188387650512141, 0.3333333333333333703, 0.3170188387650512141, 0.3333333333333333703, 0.3170188387650512141, 0.3333333333333333703, 0.3170188387650512141, 0.3333333333333333703, 0.3170188387650512141, 0.3333333333333333703, 0.3170188387650512141, 0.3333333333333333703, 0.3170188387650512141, 0.3333333333333333703, 0.3170188387650512141, 0.3333333333333333703, 0.3170188387650512141, 0.3333333333333333703, 0.3170188387650512141, 0.3333333333333333703, 0.3170188387650512141, 0.3333333333333333703, 0.3170188387650512141, 0.3333333333333333703, 0.3170188387650512141, 0.3333333333333333703, 0.3170188387650512141, 0.3333333333333333703, 0.3170188387650512141, 0.3333333333333333703, 0.3170188387650512141, 0.3333333333333333703, 0.3170188387650512141, 0.3333333333333333703, 0.3170188387650512141, 0.3333333333333333703),
 ( 1.000000000000000000, 0.9510565162951535312, 1.000000000000000000, 0.9510565162951535312, 1.000000000000000000, 0.9510565162951535312, 1.000000000000000000, 0.9510565162951535312, 1.000000000000000000, 0.9510565162951535312, 1.000000000000000000, 0.9510565162951535312, 1.000000000000000000, 0.9510565162951535312, 1.000000000000000000, 0.9510565162951535312, 1.000000000000000000, 0.9510565162951535312, 1.000000000000000000, 0.9510565162951535312, 1.000000000000000000, 0.9510565162951535312, 1.000000000000000000, 0.9510565162951535312, 1.000000000000000000, 0.9510565162951535312, 1.000000000000000000, 0.9510565162951535312, 1.000000000000000000, 0.9510565162951535312, 1.000000000000000000, 0.9510565162951535312, 1.000000000000000000, 0.9510565162951535312, 1.000000000000000000, 0.9510565162951535312, 1.000000000000000000, 0.9510565162951535312, 1.000000000000000000, 0.9510565162951535312, 1.000000000000000000, 0.9510565162951535312, 1.000000000000000000, 0.9510565162951535312, 1.000000000000000000, 0.9510565162951535312, 1.000000000000000000, 0.9510565162951535312, 1.000000000000000000, 0.9510565162951535312, 1.000000000000000000, 0.9510565162951535312, 1.000000000000000000, 0.9510565162951535312, 1.000000000000000000, 0.9510565162951535312, 1.000000000000000000, 0.9510565162951535312, 1.000000000000000000, 0.9510565162951535312, 1.000000000000000000, 0.9510565162951535312, 1.000000000000000000, 0.9510565162951535312, 1.000000000000000000, 0.9510565162951535312, 1.000000000000000000, 0.9510565162951535312, 1.000000000000000000, 0.9510565162951535312, 1.000000000000000000, 0.9510565162951535312, 1.000000000000000000, 0.9510565162951535312, 1.000000000000000000, 0.9510565162951535312, 1.000000000000000000, 0.9510565162951535312, 1.000000000000000000, 0.9510565162951535312, 1.000000000000000000, 0.9510565162951535312, 1.000000000000000000, 0.9510565162951535312, 1.000000000000000000, 0.9510565162951535312, 1.000000000000000000, 0.9510565162951535312, 1.000000000000000000, 0.9510565162951535312, 1.000000000000000000, 0.9510565162951535312, 1.000000000000000000, 0.9510565162951535312, 1.000000000000000000, 0.9510565162951535312, 1.000000000000000000, 0.9510565162951535312, 1.000000000000000000, 0.9510565162951535312, 1.000000000000000000, 0.9510565162951535312, 1.000000000000000000, 0.9510565162951535312, 1.000000000000000000, 0.9510565162951535312, 1.000000000000000000, 0.9510565162951535312, 1.000000000000000000, 0.9510565162951535312, 1.000000000000000000, 0.9510565162951535312, 1.000000000000000000, 0.9510565162951535312, 1.000000000000000000, 0.9510565162951535312, 1.000000000000000000, 0.9510565162951535312, 1.000000000000000000, 0.9510565162951535312, 1.000000000000000000, 0.9510565162951535312, 1.000000000000000000, 0.9510565162951535312, 1.000000000000000000, 0.9510565162951535312, 1.000000000000000000, 0.9510565162951535312, 1.000000000000000000, 0.9510565162951535312, 1.000000000000000000, 0.9510565162951535312, 1.000000000000000000, 0.9510565162951535312, 1.000000000000000000, 0.9510565162951535312, 1.000000000000000000, 0.9510565162951535312, 1.000000000000000000, 0.9510565162951535312, 1.000000000000000000, 0.9510565162951535312, 1.000000000000000000, 0.9510565162951535312, 1.000000000000000000, 0.9510565162951535312, 1.000000000000000000, 0.9510565162951535312, 1.000000000000000000, 0.9510565162951535312, 1.000000000000000000, 0.9510565162951535312, 1.000000000000000000, 0.9510565162951535312, 1.000000000000000000, 0.9510565162951535312, 1.000000000000000000, 0.9510565162951535312, 1.000000000000000000, 0.9510565162951535312, 1.000000000000000000, 0.9510565162951535312, 1.000000000000000000, 0.9510565162951535312, 1.000000000000000000, 0.9510565162951535312, 1.000000000000000000, 0.9510565162951535312, 1.000000000000000000, 0.9510565162951535312, 1.000000000000000000, 0.9510565162951535312, 1.000000000000000000, 0.9510565162951535312, 1.000000000000000000, 0.9510565162951535312, 1.000000000000000000, 0.9510565162951535312, 1.000000000000000000, 0.9510565162951535312, 1.000000000000000000, 0.9510565162951535312, 1.000000000000000000, 0.9510565162951535312, 1.000000000000000000, 0.9510565162951535312, 1.000000000000000000, 0.9510565162951535312, 1.000000000000000000, 0.9510565162951535312, 1.000000000000000000, 0.9510565162951535312, 1.000000000000000000, 0.9510565162951535312, 1.000000000000000000, 0.9510565162951535312, 1.000000000000000000, 0.9510565162951535312, 1.000000000000000000, 0.9510565162951535312, 1.000000000000000000, 0.9510565162951535312, 1.000000000000000000, 0.9510565162951535312, 1.000000000000000000, 0.9510565162951535312, 1.000000000000000000, 0.9510565162951535312, 1.000000000000000000, 0.9510565162951535312, 1.000000000000000000, 0.9510565162951535312, 1.000000000000000000, 0.9510565162951535312, 1.000000000000000000, 0.9510565162951535312, 1.000000000000000000, 0.9510565162951535312, 1.000000000000000000, 0.9510565162951535312, 1.000000000000000000, 0.9510565162951535312, 1.000000000000000000, 0.9510565162951535312, 1.000000000000000000, 0.9510565162951535312, 1.000000000000000000, 0.9510565162951535312, 1.000000000000000000, 0.9510565162951535312, 1.000000000000000000, 0.9510565162951535312, 1.000000000000000000, 0.9510565162951535312, 1.000000000000000000, 0.9510565162951535312, 1.000000000000000000, 0.9510565162951535312, 1.000000000000000000, 0.9510565162951535312, 1.000000000000000000, 0.9510565162951535312, 1.000000000000000000, 0.9510565162951535312, 1.000000000000000000, 0.9510565162951535312, 1.000000000000000000, 0.9510565162951535312, 1.000000000000000000, 0.9510565162951535312, 1.000000000000000000, 0.9510565162951535312, 1.000000000000000000, 0.9510565162951535312, 1.000000000000000000, 0.9510565162951535312, 1.000000000000000000, 0.9510565162951535312, 1.000000000000000000, 0.9510565162951535312, 1.000000000000000000) ) ) 
 REPRESENTATION_ITEM ( '' )  SURFACE ( )  );
#4780 = CARTESIAN_POINT ( 'NONE',  ( -4.784657899331159037, -68.89547149457074227, 1.454677039711874675 ) ) ;
#4781 = DIRECTION ( 'NONE',  ( 0.000000000000000000, -0.000000000000000000, 1.000000000000000000 ) ) ;
#4782 = CARTESIAN_POINT ( 'NONE',  ( 1.719659006605287477, -94.84547149457074511, -4.969112962950050338 ) ) ;
#4783 = CARTESIAN_POINT ( 'NONE',  ( 4.191402346623195996, -58.80452850542926058, 5.607243785695311900 ) ) ;
#4784 = VERTEX_POINT ( 'NONE', #3210 ) ;
#4785 = FACE_OUTER_BOUND ( 'NONE', #4112, .T. ) ;
#4786 = ADVANCED_FACE ( 'NONE', ( #7806 ), #6491, .F. ) ;
#4787 = VERTEX_POINT ( 'NONE', #5767 ) ;
#4788 = CARTESIAN_POINT ( 'NONE',  ( 6.123233995736760366E-16, -27.00000000000000000, 2.500000000000000888 ) ) ;
#4789 = CARTESIAN_POINT ( 'NONE',  ( -0.09506052544083921918, -84.00452850542926342, -4.999999999999997335 ) ) ;
#4790 = CARTESIAN_POINT ( 'NONE',  ( 1.529537955723689890, -74.85452850542925773, -5.030887037049978971 ) ) ;
#4791 = ORIENTED_EDGE ( 'NONE', *, *, #2637, .T. ) ;
#4792 = CARTESIAN_POINT ( 'NONE',  ( 2.862020680886513180, -68.70452850542925205, -4.100960146804039752 ) ) ;
#4793 = CARTESIAN_POINT ( 'NONE',  ( -2.823794231030039903, -77.59547149457073090, -1.017458915287723364 ) ) ;
#4794 = CARTESIAN_POINT ( 'NONE',  ( 2.493201789345307784, -60.94547149457074653, 1.934965279058241006 ) ) ;
#4795 = CARTESIAN_POINT ( 'NONE',  ( -0.09506052544084034328, -75.00452850542924921, -4.999999999999997335 ) ) ;
#4796 = CARTESIAN_POINT ( 'NONE',  ( 4.191402346623198660, -91.80452850542926058, 5.607243785695311900 ) ) ;
#4797 = CARTESIAN_POINT ( 'NONE',  ( -0.8796985632579406023, -95.14547149457074227, -3.030887037049952326 ) ) ;
#4798 = VERTEX_POINT ( 'NONE', #7083 ) ;
#4799 = CARTESIAN_POINT ( 'NONE',  ( -54.99999999999999289, -100.0000000000000000, -20.00000000000000000 ) ) ;
#4800 = ORIENTED_EDGE ( 'NONE', *, *, #7496, .T. ) ;
#4801 = CYLINDRICAL_SURFACE ( 'NONE', #3370, 3.000000000000002665 ) ;
#4802 = CARTESIAN_POINT ( 'NONE',  ( -0.09506052544081858291, -81.00452850542926342, -2.999999999999997780 ) ) ;
#4803 = CARTESIAN_POINT ( 'NONE',  ( -2.369498399071204631, -93.15452850542925489, -6.969112962950009482 ) ) ;
#4804 = CARTESIAN_POINT ( 'NONE',  ( 2.179377348189629693, -78.64547149457074227, 7.030887037049939003 ) ) ;
#4805 = DIRECTION ( 'NONE',  ( 1.000000000000000000, 9.251858538542971581E-17, 1.604941620322696727E-32 ) ) ;
#4806 = CARTESIAN_POINT ( 'NONE',  ( 4.784657899331179465, -94.39547149457074227, -1.454677039711874009 ) ) ;
#4807 = CARTESIAN_POINT ( 'NONE',  ( 3.154386672714809770, -86.25452850542924921, -0.09995255151727241993 ) ) ;
#4808 = EDGE_CURVE ( 'NONE', #2388, #3744, #7169, .T. ) ;
#4809 = STYLED_ITEM ( 'NONE', ( #7277 ), #1690 ) ;
#4810 = FILL_AREA_STYLE_COLOUR ( '', #4216 ) ;
#4811 = VERTEX_POINT ( 'NONE', #800 ) ;
#4812 = CARTESIAN_POINT ( 'NONE',  ( 6.123233995736760366E-16, -26.99999999999998934, 0.000000000000000000 ) ) ;
#4813 = CARTESIAN_POINT ( 'NONE',  ( -4.312004677471058756, -69.45452850542925205, -3.009306630940844052 ) ) ;
#4814 = CARTESIAN_POINT ( 'NONE',  ( 2.369498399071078509, -82.84547149457074511, -6.969112962950057444 ) ) ;
#4815 = ORIENTED_EDGE ( 'NONE', *, *, #6218, .T. ) ;
#4816 = CARTESIAN_POINT ( 'NONE',  ( 4.312004677471010794, -73.54547149457073374, -3.009306630940932425 ) ) ;
#4817 = CARTESIAN_POINT ( 'NONE',  ( -4.784657899331159037, -68.89547149457074227, 1.454677039711874675 ) ) ;
#4818 = CARTESIAN_POINT ( 'NONE',  ( -1.719659006605374074, -63.15452850542925489, -4.969112962950016588 ) ) ;
#4819 = LINE ( 'NONE', #1667, #6108 ) ;
#4820 = EDGE_CURVE ( 'NONE', #4058, #6070, #5138, .T. ) ;
#4821 = CARTESIAN_POINT ( 'NONE',  ( 4.725907263620372056, -73.09547149457074511, 1.635492904037598283 ) ) ;
#4822 = FACE_OUTER_BOUND ( 'NONE', #7542, .T. ) ;
#4823 = CARTESIAN_POINT ( 'NONE',  ( -6.628020296210623385, -57.90452850542925489, 2.253526892787613978 ) ) ;
#4824 = ORIENTED_EDGE ( 'NONE', *, *, #4901, .T. ) ;
#4825 = AXIS2_PLACEMENT_3D ( 'NONE', #6438, #27, #2610 ) ;
#4826 = CARTESIAN_POINT ( 'NONE',  ( 3.943604702053941724E-15, -27.99999999999999645, 0.000000000000000000 ) ) ;
#4827 = VECTOR ( 'NONE', #4906, 1000.000000000000000 ) ;
#4828 = AXIS2_PLACEMENT_3D ( 'NONE', #4342, #3621, #1843 ) ;
#4829 = EDGE_CURVE ( 'NONE', #970, #3730, #5896, .T. ) ;
#4830 = ORIENTED_EDGE ( 'NONE', *, *, #1405, .F. ) ;
#4831 = VECTOR ( 'NONE', #5098, 1000.000000000000000 ) ;
#4832 = DIRECTION ( 'NONE',  ( 0.000000000000000000, -0.7071067811865465735, 0.7071067811865485719 ) ) ;
#4833 = CARTESIAN_POINT ( 'NONE',  ( -4.725907263620319654, -90.90452850542926910, 1.635492904037698647 ) ) ;
#4834 = CARTESIAN_POINT ( 'NONE',  ( 4.194503406049337357, -74.55452850542923215, -3.171033256558100089 ) ) ;
#4835 = ORIENTED_EDGE ( 'NONE', *, *, #6258, .T. ) ;
#4836 = CARTESIAN_POINT ( 'NONE',  ( -0.09506052544084073186, -72.00452850542926342, -4.999999999999997335 ) ) ;
#4837 = CARTESIAN_POINT ( 'NONE',  ( 0.8796985632579628067, -84.64547149457074227, 3.030887037049952326 ) ) ;
#4838 = CARTESIAN_POINT ( 'NONE',  ( -4.194503406049381766, -95.44547149457071100, -3.171033256558012159 ) ) ;
#4839 = CARTESIAN_POINT ( 'NONE',  ( 4.312004677471076519, -79.95452850542922363, 3.009306630940844496 ) ) ;
#4840 = AXIS2_PLACEMENT_3D ( 'NONE', #3925, #5225, #5945 ) ;
#4841 = CARTESIAN_POINT ( 'NONE',  ( 4.037591185471444355, -89.70452850542925205, -5.718994135553947977 ) ) ;
#4842 = CARTESIAN_POINT ( 'NONE',  ( -1.686450176301567572, -61.20452850542925916, 2.482926158054133303 ) ) ;
#4843 = SHAPE_DEFINITION_REPRESENTATION ( #1859, #153 ) ;
#4844 = ADVANCED_FACE ( 'NONE', ( #1954, #128, #5855 ), #5269, .T. ) ;
#4845 = VERTEX_POINT ( 'NONE', #7763 ) ;
#4846 = PLANE ( 'NONE',  #255 ) ;
#4847 = MECHANICAL_DESIGN_GEOMETRIC_PRESENTATION_REPRESENTATION (  '', ( #6998 ), #3909 ) ;
#4848 = DIRECTION ( 'NONE',  ( -0.000000000000000000, 0.000000000000000000, 1.000000000000000000 ) ) ;
#4849 = CARTESIAN_POINT ( 'NONE',  ( -2.823794231030022139, -66.90452850542925489, 1.017458915287783316 ) ) ;
#4850 = EDGE_CURVE ( 'NONE', #3416, #2326, #6986, .T. ) ;
#4851 = CARTESIAN_POINT ( 'NONE',  ( 0.09506052544073424759, -76.99547149457075079, -6.999999999999997335 ) ) ;
#4852 = DIRECTION ( 'NONE',  ( 0.000000000000000000, -1.000000000000000000, 0.000000000000000000 ) ) ;
#4853 = CARTESIAN_POINT ( 'NONE',  ( 55.00000000000000000, -25.00000000000002132, -20.00000000000000000 ) ) ;
#4854 = STYLED_ITEM ( 'NONE', ( #3552 ), #3582 ) ;
#4855 = CARTESIAN_POINT ( 'NONE',  ( -2.823794231030019919, -84.90452850542926910, 1.017458915287783316 ) ) ;
#4856 = UNCERTAINTY_MEASURE_WITH_UNIT (LENGTH_MEASURE( 1.000000000000000082E-05 ), #2005, 'distance_accuracy_value', 'NONE');
#4857 =( LENGTH_UNIT ( ) NAMED_UNIT ( * ) SI_UNIT ( .MILLI., .METRE. ) );
#4858 = ORIENTED_EDGE ( 'NONE', *, *, #3004, .F. ) ;
#4859 = PLANE ( 'NONE',  #4354 ) ;
#4860 = CARTESIAN_POINT ( 'NONE',  ( 3.015831842038231958, -61.80452850542926058, 3.989209796945429432 ) ) ;
#4861 = CARTESIAN_POINT ( 'NONE',  ( 4.037591185471561595, -72.79547149457074795, 5.718994135553860936 ) ) ;
#4862 =( NAMED_UNIT ( * ) PLANE_ANGLE_UNIT ( ) SI_UNIT ( $, .RADIAN. ) );
#4863 = ORIENTED_EDGE ( 'NONE', *, *, #5085, .T. ) ;
#4864 = EDGE_CURVE ( 'NONE', #524, #6860, #4544, .T. ) ;
#4865 = CARTESIAN_POINT ( 'NONE',  ( -1.529537955723777598, -74.14547149457074227, -5.030887037049945221 ) ) ;
#4866 = CARTESIAN_POINT ( 'NONE',  ( 1.529537955723795140, -72.64547149457075648, 5.030887037049945221 ) ) ;
#4867 = CARTESIAN_POINT ( 'NONE',  ( 1.529537955723689224, -68.85452850542921510, -5.030887037049978971 ) ) ;
#4868 = DIRECTION ( 'NONE',  ( 0.000000000000000000, -0.7071067811865507924, 0.7071067811865441310 ) ) ;
#4869 =( REPRESENTATION_RELATIONSHIP ('NONE','NONE', #4188, #1019 ) REPRESENTATION_RELATIONSHIP_WITH_TRANSFORMATION ( #8321 )SHAPE_REPRESENTATION_RELATIONSHIP( ) );
#4870 = CARTESIAN_POINT ( 'NONE',  ( 4.194503406049400418, -66.94547149457075363, 3.171033256558012159 ) ) ;
#4871 =( NAMED_UNIT ( * ) PLANE_ANGLE_UNIT ( ) SI_UNIT ( $, .RADIAN. ) );
#4872 = CARTESIAN_POINT ( 'NONE',  ( 2.862020680886516732, -95.70452850542926626, -4.100960146804039752 ) ) ;
#4873 = ORIENTED_EDGE ( 'NONE', *, *, #3976, .F. ) ;
#4874 = DIRECTION ( 'NONE',  ( 1.000000000000000000, 0.000000000000000000, 0.000000000000000000 ) ) ;
#4875 = PRODUCT ( 'pin 2', 'pin 2', '', ( #4205 ) ) ;
#4876 = VERTEX_POINT ( 'NONE', #3299 ) ;
#4877 = DIRECTION ( 'NONE',  ( -1.000000000000000000, 0.000000000000000000, 0.000000000000000000 ) ) ;
#4878 = CARTESIAN_POINT ( 'NONE',  ( -4.725907263620319654, -87.90452850542926910, 1.635492904037698647 ) ) ;
#4879 = CARTESIAN_POINT ( 'NONE',  ( 4.312004677471075631, -76.95452850542923784, 3.009306630940844496 ) ) ;
#4880 = CARTESIAN_POINT ( 'NONE',  ( 3.015831842038231958, -58.80452850542925347, 3.989209796945429432 ) ) ;
#4881 = CARTESIAN_POINT ( 'NONE',  ( 0.8796985632579621406, -78.64547149457074227, 3.030887037049952326 ) ) ;
#4882 = CARTESIAN_POINT ( 'NONE',  ( 4.312004677471013459, -97.54547149457070532, -3.009306630940933314 ) ) ;
#4883 = CARTESIAN_POINT ( 'NONE',  ( 4.784657899331208775, -71.10452850542925773, 1.454677039711774533 ) ) ;
#4884 = CARTESIAN_POINT ( 'NONE',  ( -2.179377348189460051, -88.35452850542924352, 7.030887037049988741 ) ) ;
#4885 = CARTESIAN_POINT ( 'NONE',  ( -2.882544866740879730, -57.60452850542926484, -0.8366430509618996147 ) ) ;
#4886 = APPLICATION_PROTOCOL_DEFINITION ( 'draft international standard', 'automotive_design', 1998, #2019 ) ;
#4887 = VERTEX_POINT ( 'NONE', #6575 ) ;
#4888 = CARTESIAN_POINT ( 'NONE',  ( 6.000000000000006217, -51.00000000000000711, -2.499999999999999112 ) ) ;
#4889 = ORIENTED_EDGE ( 'NONE', *, *, #4722, .F. ) ;
#4890 = LINE ( 'NONE', #2834, #1206 ) ;
#4891 = CARTESIAN_POINT ( 'NONE',  ( 1.686450176301584003, -65.70452850542925205, -2.482926158054133303 ) ) ;
#4892 = CIRCLE ( 'NONE', #1256, 3.000000000000000000 ) ;
#4893 = CARTESIAN_POINT ( 'NONE',  ( -4.037591185471544719, -77.29547149457074795, -5.718994135553860936 ) ) ;
#4894 = CARTESIAN_POINT ( 'NONE',  ( 6.123233995736760366E-16, -27.00000000000000000, 2.500000000000000888 ) ) ;
#4895 = EDGE_CURVE ( 'NONE', #4784, #3705, #1393, .T. ) ;
#4896 = CARTESIAN_POINT ( 'NONE',  ( -4.725907263620351628, -92.59547149457074511, -1.635492904037597617 ) ) ;
#4897 = CARTESIAN_POINT ( 'NONE',  ( -3.154386672714787565, -87.75452850542924921, 0.09995255151727280851 ) ) ;
#4898 = VECTOR ( 'NONE', #7708, 1000.000000000000000 ) ;
#4899 =( LENGTH_UNIT ( ) NAMED_UNIT ( * ) SI_UNIT ( .MILLI., .METRE. ) );
#4900 = EDGE_LOOP ( 'NONE', ( #6331, #4087, #8057, #8252 ) ) ;
#4901 = EDGE_CURVE ( 'NONE', #2153, #6782, #7677, .T. ) ;
#4902 = DIRECTION ( 'NONE',  ( 9.251858538542971581E-17, -1.000000000000000000, 0.000000000000000000 ) ) ;
#4903 = CARTESIAN_POINT ( 'NONE',  ( 0.8796985632579009673, -92.85452850542924352, -3.030887037049972310 ) ) ;
#4904 = CARTESIAN_POINT ( 'NONE',  ( -0.09506052544071416643, -75.49547149457075079, 6.999999999999997335 ) ) ;
#4905 = SHAPE_REPRESENTATION_RELATIONSHIP ( 'NONE' , 'NONE' ,  #1613, #2890 ) ;
#4906 = DIRECTION ( 'NONE',  ( -0.000000000000000000, 0.7071067811865484609, 0.7071067811865465735 ) ) ;
#4907 = CARTESIAN_POINT ( 'NONE',  ( 1.719659006605285922, -76.84547149457071669, -4.969112962950050338 ) ) ;
#4908 = CARTESIAN_POINT ( 'NONE',  ( 0.09506052544075450916, -70.99547149457075079, -4.999999999999997335 ) ) ;
#4909 = VECTOR ( 'NONE', #5698, 1000.000000000000000 ) ;
#4910 = CARTESIAN_POINT ( 'NONE',  ( 4.784657899331208775, -68.10452850542925773, 1.454677039711774533 ) ) ;
#4911 = CARTESIAN_POINT ( 'NONE',  ( 80.00000000000000000, -9.999999999999994671, 10.50000000000000533 ) ) ;
#4912 = CARTESIAN_POINT ( 'NONE',  ( -3.015831842038130706, -63.19547149457074653, 3.989209796945492048 ) ) ;
#4913 =( NAMED_UNIT ( * ) SI_UNIT ( $, .STERADIAN. ) SOLID_ANGLE_UNIT ( ) );
#4914 = CARTESIAN_POINT ( 'NONE',  ( 0.09506052544086235345, -94.50452850542926342, 4.999999999999997335 ) ) ;
#4915 = ORIENTED_EDGE ( 'NONE', *, *, #4722, .T. ) ;
#4916 = CARTESIAN_POINT ( 'NONE',  ( 50.00000000000000000, -1.734723475976807094E-15, 12.50000000000000000 ) ) ;
#4917 = ORIENTED_EDGE ( 'NONE', *, *, #7070, .T. ) ;
#4918 = FACE_OUTER_BOUND ( 'NONE', #3055, .T. ) ;
#4919 = CARTESIAN_POINT ( 'NONE',  ( 4.194503406049338246, -83.55452850542921794, -3.171033256558100089 ) ) ;
#4920 = CARTESIAN_POINT ( 'NONE',  ( 5.257311121191342806, -91.24547149457072237, 0.09995255151718437925 ) ) ;
#4921 = CARTESIAN_POINT ( 'NONE',  ( 4.312004677471074743, -64.95452850542926626, 3.009306630940844052 ) ) ;
#4922 = CARTESIAN_POINT ( 'NONE',  ( 3.154386672714809770, -82.24547149457073658, 0.09995255151720662534 ) ) ;
#4923 = CARTESIAN_POINT ( 'NONE',  ( 3.015831842038149802, -85.69547149457073942, -3.989209796945492048 ) ) ;
#4924 = CARTESIAN_POINT ( 'NONE',  ( -0.09506052544084148126, -66.00452850542926342, -4.999999999999997335 ) ) ;
#4925 = CARTESIAN_POINT ( 'NONE',  ( 6.013306294175169597, -82.95452850542925205, 4.245374608440616093 ) ) ;
#4926 = EDGE_CURVE ( 'NONE', #7486, #3662, #6046, .T. ) ;
#4927 = CARTESIAN_POINT ( 'NONE',  ( 3.154386672714811102, -94.24547149457075079, 0.09995255151720662534 ) ) ;
#4928 = VERTEX_POINT ( 'NONE', #4799 ) ;
#4929 = DIRECTION ( 'NONE',  ( 1.000000000000000000, 0.000000000000000000, 0.000000000000000000 ) ) ;
#4930 = ORIENTED_EDGE ( 'NONE', *, *, #991, .F. ) ;
#4931 = CARTESIAN_POINT ( 'NONE',  ( 4.194503406049340022, -86.55452850542926058, -3.171033256558100977 ) ) ;
#4932 = CARTESIAN_POINT ( 'NONE',  ( 3.154386672714808437, -71.25452850542926342, -0.09995255151727241993 ) ) ;
#4933 = CARTESIAN_POINT ( 'NONE',  ( -7.360235569667858968, -77.74547149457073658, -0.09995255151716124498 ) ) ;
#4934 = CARTESIAN_POINT ( 'NONE',  ( -4.312004677471055203, -93.45452850542922363, -3.009306630940844052 ) ) ;
#4935 = CARTESIAN_POINT ( 'NONE',  ( -3.015831842038126709, -96.19547149457075363, 3.989209796945492048 ) ) ;
#4936 = CARTESIAN_POINT ( 'NONE',  ( 1.840261337453272583, -88.80452850542926058, 2.371175808195547852 ) ) ;
#4937 = LINE ( 'NONE', #3635, #2550 ) ;
#4938 = ORIENTED_EDGE ( 'NONE', *, *, #1855, .F. ) ;
#4939 = CARTESIAN_POINT ( 'NONE',  ( -4.194503406049321370, -58.05452850542925347, 3.171033256558100533 ) ) ;
#4940 = CARTESIAN_POINT ( 'NONE',  ( 6.686770931921476979, -67.39547149457074227, -2.072711028461788896 ) ) ;
#4941 = CARTESIAN_POINT ( 'NONE',  ( -65.00000000000000000, -9.999999999999994671, 10.50000000000000533 ) ) ;
#4942 = CARTESIAN_POINT ( 'NONE',  ( -4.725907263620354293, -71.59547149457074511, -1.635492904037597617 ) ) ;
#4943 = CARTESIAN_POINT ( 'NONE',  ( 1.529537955723795140, -69.64547149457074227, 5.030887037049945221 ) ) ;
#4944 = CARTESIAN_POINT ( 'NONE',  ( 1.069819614139559061, -94.65452850542924068, 2.969112962950023249 ) ) ;
#4945 = CARTESIAN_POINT ( 'NONE',  ( 75.00000000000000000, 80.00000000000000000, 7.500000000000000000 ) ) ;
#4946 = CARTESIAN_POINT ( 'NONE',  ( 2.862020680886512736, -65.70452850542925205, -4.100960146804039752 ) ) ;
#4947 = CARTESIAN_POINT ( 'NONE',  ( -1.719659006605267937, -60.34547149457073090, 4.969112962950051227 ) ) ;
#4948 = ORIENTED_EDGE ( 'NONE', *, *, #6418, .F. ) ;
#4949 = CARTESIAN_POINT ( 'NONE',  ( 0.000000000000000000, 0.000000000000000000, -7.500000000000000000 ) ) ;
#4950 = EDGE_LOOP ( 'NONE', ( #7754, #4219, #7967, #3648 ) ) ;
#4951 = FACE_BOUND ( 'NONE', #5931, .T. ) ;
#4952 = CARTESIAN_POINT ( 'NONE',  ( 1.529537955723690557, -80.85452850542925773, -5.030887037049978971 ) ) ;
#4953 = CARTESIAN_POINT ( 'NONE',  ( 0.09506052544075639654, -85.99547149457075079, -4.999999999999997335 ) ) ;
#4954 = EDGE_CURVE ( 'NONE', #6070, #417, #6069, .T. ) ;
#4955 = CARTESIAN_POINT ( 'NONE',  ( -4.194503406049320482, -64.05452850542926058, 3.171033256558101865 ) ) ;
#4956 = CARTESIAN_POINT ( 'NONE',  ( -3.154386672714789341, -80.74547149457075079, -0.09995255151720625064 ) ) ;
#4957 = CARTESIAN_POINT ( 'NONE',  ( 4.037591185471443467, -83.70452850542925205, -5.718994135553947977 ) ) ;
#4958 = CARTESIAN_POINT ( 'NONE',  ( -0.09506052544073428923, -84.49547149457075079, 4.999999999999997335 ) ) ;
#4959 = CARTESIAN_POINT ( 'NONE',  ( 0.09506052544085895339, -67.50452850542926342, 4.999999999999997335 ) ) ;
#4960 = CARTESIAN_POINT ( 'NONE',  ( -4.191402346623178232, -81.30452850542926058, -5.607243785695311900 ) ) ;
#4961 = CARTESIAN_POINT ( 'NONE',  ( -1.686450176301615977, -86.29547149457074795, -2.482926158054096000 ) ) ;
#4962 = AXIS2_PLACEMENT_3D ( 'NONE', #2715, #5273, #7767 ) ;
#4963 = CIRCLE ( 'NONE', #5632, 6.000000000000000000 ) ;
#4964 = ORIENTED_EDGE ( 'NONE', *, *, #7749, .T. ) ;
#4965 = DIRECTION ( 'NONE',  ( 0.000000000000000000, 0.000000000000000000, -1.000000000000000000 ) ) ;
#4966 = ORIENTED_EDGE ( 'NONE', *, *, #2919, .T. ) ;
#4967 = CARTESIAN_POINT ( 'NONE',  ( -5.257311121191322378, -90.75452850542924921, 0.09995255151729529053 ) ) ;
#4968 = CARTESIAN_POINT ( 'NONE',  ( -0.8796985632578808723, -64.35452850542924352, 3.030887037049973198 ) ) ;
#4969 =( GEOMETRIC_REPRESENTATION_CONTEXT ( 3 ) GLOBAL_UNCERTAINTY_ASSIGNED_CONTEXT ( ( #2842 ) ) GLOBAL_UNIT_ASSIGNED_CONTEXT ( ( #6571, #6444, #7758 ) ) REPRESENTATION_CONTEXT ( 'NONE', 'WORKASPACE' ) );
#4970 = CARTESIAN_POINT ( 'NONE',  ( -4.191402346623180897, -60.30452850542926058, -5.607243785695311900 ) ) ;
#4971 = CARTESIAN_POINT ( 'NONE',  ( -6.013306294175061240, -72.04547149457074795, 4.245374608440741326 ) ) ;
#4972 = FACE_OUTER_BOUND ( 'NONE', #383, .T. ) ;
#4973 = CARTESIAN_POINT ( 'NONE',  ( -1.719659006605264384, -87.34547149457074511, 4.969112962950051227 ) ) ;
#4974 = CARTESIAN_POINT ( 'NONE',  ( 2.882544866740897049, -83.10452850542927195, 0.8366430509618999478 ) ) ;
#4975 = AXIS2_PLACEMENT_3D ( 'NONE', #4692, #4109, #7954 ) ;
#4976 = VERTEX_POINT ( 'NONE', #4089 ) ;
#4977 = SURFACE_STYLE_USAGE ( .BOTH. , #8186 ) ;
#4978 = CARTESIAN_POINT ( 'NONE',  ( -4.725907263620323207, -60.90452850542925489, 1.635492904037698647 ) ) ;
#4979 = CARTESIAN_POINT ( 'NONE',  ( -6.628020296210667794, -68.59547149457073090, -2.253526892787471869 ) ) ;
#4980 = FILL_AREA_STYLE_COLOUR ( '', #4026 ) ;
#4981 = CARTESIAN_POINT ( 'NONE',  ( 6.123233995736760366E-16, -27.00000000000000000, 5.000000000000000000 ) ) ;
#4982 =( GEOMETRIC_REPRESENTATION_CONTEXT ( 3 ) GLOBAL_UNCERTAINTY_ASSIGNED_CONTEXT ( ( #2352 ) ) GLOBAL_UNIT_ASSIGNED_CONTEXT ( ( #1034, #5538, #4311 ) ) REPRESENTATION_CONTEXT ( 'NONE', 'WORKASPACE' ) );
#4983 = CARTESIAN_POINT ( 'NONE',  ( -3.015831842038129817, -69.19547149457073942, 3.989209796945492048 ) ) ;
#4984 = CARTESIAN_POINT ( 'NONE',  ( -1.529537955723777820, -68.14547149457075648, -5.030887037049945221 ) ) ;
#4985 = CARTESIAN_POINT ( 'NONE',  ( 4.194503406049334693, -59.55452850542926058, -3.171033256558100089 ) ) ;
#4986 = FACE_OUTER_BOUND ( 'NONE', #2783, .T. ) ;
#4987 = CARTESIAN_POINT ( 'NONE',  ( -3.015831842038215971, -69.30452850542926058, -3.989209796945429432 ) ) ;
#4988 = CARTESIAN_POINT ( 'NONE',  ( -1.719659006605267493, -63.34547149457075221, 4.969112962950051227 ) ) ;
#4989 =( NAMED_UNIT ( * ) PLANE_ANGLE_UNIT ( ) SI_UNIT ( $, .RADIAN. ) );
#4990 = ORIENTED_EDGE ( 'NONE', *, *, #1426, .T. ) ;
#4991 = CARTESIAN_POINT ( 'NONE',  ( 65.00000000000000000, -12.00000000000000711, 12.49999999999999822 ) ) ;
#4992 = EDGE_CURVE ( 'NONE', #6465, #140, #7422, .T. ) ;
#4993 = VERTEX_POINT ( 'NONE', #6027 ) ;
#4994 = CARTESIAN_POINT ( 'NONE',  ( -0.1932469879202498297, -30.15636746936407064, 2.500000000000000888 ) ) ;
#4995 = CARTESIAN_POINT ( 'NONE',  ( -2.862020680886494972, -73.20452850542925205, 4.100960146804039752 ) ) ;
#4996 = CARTESIAN_POINT ( 'NONE',  ( 1.529537955723797138, -93.64547149457074227, 5.030887037049945221 ) ) ;
#4997 = CARTESIAN_POINT ( 'NONE',  ( 2.862020680886511848, -59.70452850542925205, -4.100960146804039752 ) ) ;
#4998 = CARTESIAN_POINT ( 'NONE',  ( -0.09506052544075668798, -75.49547149457075079, 2.999999999999997780 ) ) ;
#4999 = CARTESIAN_POINT ( 'NONE',  ( 0.09506052544088175460, -79.50452850542926342, 6.999999999999997335 ) ) ;
#5000 = CARTESIAN_POINT ( 'NONE',  ( 4.194503406049402194, -90.94547149457071100, 3.171033256558012159 ) ) ;
#5001 = CARTESIAN_POINT ( 'NONE',  ( -2.862020680886495860, -64.20452850542926626, 4.100960146804039752 ) ) ;
#5002 = CARTESIAN_POINT ( 'NONE',  ( -2.179377348189461827, -76.35452850542924352, 7.030887037049988741 ) ) ;
#5003 = CARTESIAN_POINT ( 'NONE',  ( 1.069819614139496000, -91.84547149457074511, -2.969112962950042789 ) ) ;
#5004 = VERTEX_POINT ( 'NONE', #7374 ) ;
#5005 = CARTESIAN_POINT ( 'NONE',  ( 6.123233995736760366E-16, -27.00000000000000000, 5.000000000000000000 ) ) ;
#5006 = FACE_BOUND ( 'NONE', #2334, .T. ) ;
#5007 = ORIENTED_EDGE ( 'NONE', *, *, #8335, .F. ) ;
#5008 = CARTESIAN_POINT ( 'NONE',  ( -4.784657899331189235, -87.60452850542925773, -1.454677039711773867 ) ) ;
#5009 = CARTESIAN_POINT ( 'NONE',  ( -1.840261337453252821, -66.30452850542926058, -2.371175808195547852 ) ) ;
#5010 = CARTESIAN_POINT ( 'NONE',  ( 5.257311121191343695, -95.25452850542924921, -0.09995255151729465215 ) ) ;
#5011 = EDGE_CURVE ( 'NONE', #1658, #2259, #7123, .T. ) ;
#5012 = CARTESIAN_POINT ( 'NONE',  ( -6.686770931921459216, -68.89547149457074227, 2.072711028461789784 ) ) ;
#5013 = CARTESIAN_POINT ( 'NONE',  ( -4.725907263620351628, -89.59547149457074511, -1.635492904037597617 ) ) ;
#5014 = CARTESIAN_POINT ( 'NONE',  ( 2.610703060766983885, -76.95452850542926626, 1.773238653441072232 ) ) ;
#5015 = DIRECTION ( 'NONE',  ( -1.000000000000000000, 0.000000000000000000, 0.000000000000000000 ) ) ;
#5016 = ORIENTED_EDGE ( 'NONE', *, *, #7223, .F. ) ;
#5017 = DIRECTION ( 'NONE',  ( 0.000000000000000000, -0.7071067811865507924, 0.7071067811865441310 ) ) ;
#5018 = CARTESIAN_POINT ( 'NONE',  ( 1.529537955723688780, -62.85452850542925063, -5.030887037049978971 ) ) ;
#5019 = CARTESIAN_POINT ( 'NONE',  ( -6.686770931921459216, -74.89547149457074227, 2.072711028461789784 ) ) ;
#5020 = APPLICATION_CONTEXT ( 'automotive_design' ) ;
#5021 = PLANE ( 'NONE',  #7396 ) ;
#5022 = CARTESIAN_POINT ( 'NONE',  ( -1.719659006605267049, -66.34547149457073090, 4.969112962950051227 ) ) ;
#5023 = CARTESIAN_POINT ( 'NONE',  ( 5.257311121191341918, -61.24547149457074369, 0.09995255151718437925 ) ) ;
#5024 = CARTESIAN_POINT ( 'NONE',  ( -2.610703060766962569, -90.45452850542926626, -1.773238653441072232 ) ) ;
#5025 = CARTESIAN_POINT ( 'NONE',  ( 43.45299461620744097, 100.0000000000000000, 7.500000000000000000 ) ) ;
#5026 = EDGE_CURVE ( 'NONE', #3622, #2855, #6147, .T. ) ;
#5027 = PRESENTATION_LAYER_ASSIGNMENT (  '', '', ( #7050 ) ) ;
#5028 = AXIS2_PLACEMENT_3D ( 'NONE', #6973, #2511, #1208 ) ;
#5029 = CARTESIAN_POINT ( 'NONE',  ( -4.784657899331191011, -66.60452850542924352, -1.454677039711773867 ) ) ;
#5030 = CARTESIAN_POINT ( 'NONE',  ( -1.529537955723778042, -65.14547149457074227, -5.030887037049945221 ) ) ;
#5031 = VECTOR ( 'NONE', #3811, 1000.000000000000000 ) ;
#5032 = VERTEX_POINT ( 'NONE', #844 ) ;
#5033 = CARTESIAN_POINT ( 'NONE',  ( 47.49999999999999289, -198.2344135219424857, 12.49999999999993960 ) ) ;
#5034 = VECTOR ( 'NONE', #6010, 1000.000000000000000 ) ;
#5035 = EDGE_LOOP ( 'NONE', ( #7861, #3138, #3471, #3103 ) ) ;
#5036 = PLANE ( 'NONE',  #3009 ) ;
#5037 = CARTESIAN_POINT ( 'NONE',  ( -3.015831842038214194, -81.30452850542926058, -3.989209796945429432 ) ) ;
#5038 = CARTESIAN_POINT ( 'NONE',  ( -1.529537955723775156, -89.14547149457074227, -5.030887037049945221 ) ) ;
#5039 = CLOSED_SHELL ( 'NONE', ( #7731, #7441, #5065, #2521 ) ) ;
#5040 = CARTESIAN_POINT ( 'NONE',  ( -1.719659006605373630, -66.15452850542925489, -4.969112962950015699 ) ) ;
#5041 = CARTESIAN_POINT ( 'NONE',  ( 0.8796985632579604752, -66.64547149457072805, 3.030887037049952326 ) ) ;
#5042 = CARTESIAN_POINT ( 'NONE',  ( 2.179377348189482699, -83.85452850542927195, -7.030887037049986077 ) ) ;
#5043 = CARTESIAN_POINT ( 'NONE',  ( 1.719659006605286367, -85.84547149457075932, -4.969112962950050338 ) ) ;
#5044 = LINE ( 'NONE', #5749, #2134 ) ;
#5045 = CARTESIAN_POINT ( 'NONE',  ( -5.895805022753386027, -79.05452850542926058, 4.407101234057909878 ) ) ;
#5046 = CARTESIAN_POINT ( 'NONE',  ( -1.686450176301614867, -92.29547149457074795, -2.482926158054096000 ) ) ;
#5047 = ORIENTED_EDGE ( 'NONE', *, *, #4767, .F. ) ;
#5048 = CARTESIAN_POINT ( 'NONE',  ( 54.99999999999999289, -9.999999999999994671, 1.500000000000000666 ) ) ;
#5049 = LINE ( 'NONE', #3831, #6775 ) ;
#5050 = ORIENTED_EDGE ( 'NONE', *, *, #5995, .T. ) ;
#5051 = CARTESIAN_POINT ( 'NONE',  ( -4.194503406049315153, -94.05452850542926058, 3.171033256558101865 ) ) ;
#5052 = CARTESIAN_POINT ( 'NONE',  ( -0.8796985632578817604, -58.35452850542927195, 3.030887037049973198 ) ) ;
#5053 = CARTESIAN_POINT ( 'NONE',  ( 4.725907263620341858, -92.40452850542925489, -1.635492904037697981 ) ) ;
#5054 = CARTESIAN_POINT ( 'NONE',  ( -6.686770931921459216, -71.89547149457074227, 2.072711028461789784 ) ) ;
#5055 = CARTESIAN_POINT ( 'NONE',  ( 1.719659006605287255, -88.84547149457073090, -4.969112962950050338 ) ) ;
#5056 = CARTESIAN_POINT ( 'NONE',  ( 2.823794231030040791, -77.40452850542925489, -1.017458915287783316 ) ) ;
#5057 = CARTESIAN_POINT ( 'NONE',  ( -55.00000000000000000, -25.00000000000002132, 20.00000000000000000 ) ) ;
#5058 = ORIENTED_EDGE ( 'NONE', *, *, #806, .F. ) ;
#5059 = CARTESIAN_POINT ( 'NONE',  ( 3.154386672714809770, -83.25452850542926342, -0.09995255151727241993 ) ) ;
#5060 = CARTESIAN_POINT ( 'NONE',  ( -6.013306294175061240, -63.04547149457074084, 4.245374608440741326 ) ) ;
#5061 = LINE ( 'NONE', #1192, #1604 ) ;
#5062 = CARTESIAN_POINT ( 'NONE',  ( 4.312004677471009906, -61.54547149457073374, -3.009306630940932425 ) ) ;
#5063 = CARTESIAN_POINT ( 'NONE',  ( -1.529537955723778930, -59.14547149457072805, -5.030887037049945221 ) ) ;
#5064 = CARTESIAN_POINT ( 'NONE',  ( 2.610703060766986106, -94.95452850542926626, 1.773238653441072232 ) ) ;
#5065 = ADVANCED_FACE ( 'NONE', ( #4168 ), #333, .T. ) ;
#5066 = DIRECTION ( 'NONE',  ( 1.000000000000000000, 0.000000000000000000, 0.000000000000000000 ) ) ;
#5067 = CARTESIAN_POINT ( 'NONE',  ( 4.194503406049335581, -71.55452850542926058, -3.171033256558100089 ) ) ;
#5068 = CARTESIAN_POINT ( 'NONE',  ( 4.037591185471565147, -96.79547149457073374, 5.718994135553860936 ) ) ;
#5069 = SHAPE_REPRESENTATION_RELATIONSHIP ( 'NONE' , 'NONE' ,  #1019, #7608 ) ;
#5070 = VERTEX_POINT ( 'NONE', #1647 ) ;
#5071 = DIRECTION ( 'NONE',  ( -1.000000000000000000, -1.261617073437677752E-16, 0.000000000000000000 ) ) ;
#5072 =( NAMED_UNIT ( * ) PLANE_ANGLE_UNIT ( ) SI_UNIT ( $, .RADIAN. ) );
#5073 = AXIS2_PLACEMENT_3D ( 'NONE', #5082, #5793, #7662 ) ;
#5074 = EDGE_LOOP ( 'NONE', ( #2255, #2093 ) ) ;
#5075 = DIRECTION ( 'NONE',  ( 0.000000000000000000, -1.000000000000000000, 0.000000000000000000 ) ) ;
#5076 = CARTESIAN_POINT ( 'NONE',  ( 2.862020680886514068, -74.70452850542926626, -4.100960146804039752 ) ) ;
#5077 = CARTESIAN_POINT ( 'NONE',  ( 4.725907263620373833, -85.09547149457074511, 1.635492904037598283 ) ) ;
#5078 = CARTESIAN_POINT ( 'NONE',  ( 4.371993031763548032, -96.99999999999994316, 1.072437430859429552 ) ) ;
#5079 = CARTESIAN_POINT ( 'NONE',  ( 2.610703060766944805, -73.54547149457074795, -1.773238653441125523 ) ) ;
#5080 = CARTESIAN_POINT ( 'NONE',  ( -0.09506052544086139588, -75.00452850542926342, -6.999999999999997335 ) ) ;
#5081 = CARTESIAN_POINT ( 'NONE',  ( -0.09506052544073352595, -90.49547149457073658, 4.999999999999997335 ) ) ;
#5082 = CARTESIAN_POINT ( 'NONE',  ( 65.00000000000000000, 0.000000000000000000, 0.000000000000000000 ) ) ;
#5083 = CARTESIAN_POINT ( 'NONE',  ( 6.013306294175169597, -76.95452850542926626, 4.245374608440616093 ) ) ;
#5084 = CARTESIAN_POINT ( 'NONE',  ( -2.823794231030038571, -92.59547149457074511, -1.017458915287723364 ) ) ;
#5085 = EDGE_CURVE ( 'NONE', #8159, #6872, #2161, .T. ) ;
#5086 = ORIENTED_EDGE ( 'NONE', *, *, #2429, .F. ) ;
#5087 = DIRECTION ( 'NONE',  ( 1.000000000000000000, 0.000000000000000000, 0.000000000000000000 ) ) ;
#5088 = CARTESIAN_POINT ( 'NONE',  ( 50.00000000000000000, -9.999999999999991118, 9.499999999999998224 ) ) ;
#5089 = ORIENTED_EDGE ( 'NONE', *, *, #5458, .F. ) ;
#5090 = CARTESIAN_POINT ( 'NONE',  ( 5.257311121191343695, -86.25452850542924921, -0.09995255151729466603 ) ) ;
#5091 = CARTESIAN_POINT ( 'NONE',  ( -2.823794231030023472, -57.90452850542925489, 1.017458915287783316 ) ) ;
#5092 = CARTESIAN_POINT ( 'NONE',  ( -4.784657899331188347, -93.60452850542925773, -1.454677039711773867 ) ) ;
#5093 = CARTESIAN_POINT ( 'NONE',  ( -4.191402346623060104, -66.19547149457073942, 5.607243785695398941 ) ) ;
#5094 = VECTOR ( 'NONE', #7623, 1000.000000000000000 ) ;
#5095 = CARTESIAN_POINT ( 'NONE',  ( -2.862020680886579349, -86.29547149457074795, -4.100960146803977580 ) ) ;
#5096 = CARTESIAN_POINT ( 'NONE',  ( 0.8796985632578991909, -77.85452850542925773, -3.030887037049972310 ) ) ;
#5097 = ADVANCED_FACE ( 'NONE', ( #888 ), #5311, .F. ) ;
#5098 = DIRECTION ( 'NONE',  ( 1.000000000000000000, 0.000000000000000000, 0.000000000000000000 ) ) ;
#5099 = MECHANICAL_DESIGN_GEOMETRIC_PRESENTATION_REPRESENTATION (  '', ( #3627 ), #4969 ) ;
#5100 = CARTESIAN_POINT ( 'NONE',  ( 2.882544866740898382, -89.10452850542925773, 0.8366430509618999478 ) ) ;
#5101 = PRESENTATION_LAYER_ASSIGNMENT (  '', '', ( #7261 ) ) ;
#5102 = CARTESIAN_POINT ( 'NONE',  ( 6.686770931921525829, -95.10452850542925773, 2.072711028461649008 ) ) ;
#5103 = CARTESIAN_POINT ( 'NONE',  ( -55.00000000000000000, -25.00000000000002132, -20.00000000000000000 ) ) ;
#5104 = CARTESIAN_POINT ( 'NONE',  ( -0.09506052544073655131, -66.49547149457075079, 4.999999999999997335 ) ) ;
#5105 = CARTESIAN_POINT ( 'NONE',  ( 1.529537955723793585, -60.64547149457074937, 5.030887037049945221 ) ) ;
#5106 = CARTESIAN_POINT ( 'NONE',  ( 1.069819614139558839, -91.65452850542924068, 2.969112962950023249 ) ) ;
#5107 = CARTESIAN_POINT ( 'NONE',  ( 45.00000000000000000, -14.99999999999999112, 9.500000000000000000 ) ) ;
#5108 = VECTOR ( 'NONE', #4757, 1000.000000000000000 ) ;
#5109 = CARTESIAN_POINT ( 'NONE',  ( -1.719659006605373630, -66.15452850542926910, -4.969112962950016588 ) ) ;
#5110 = EDGE_CURVE ( 'NONE', #6264, #6149, #4153, .T. ) ;
#5111 = CARTESIAN_POINT ( 'NONE',  ( -7.360235569667856304, -92.74547149457073658, -0.09995255151716124498 ) ) ;
#5112 = VERTEX_POINT ( 'NONE', #3423 ) ;
#5113 = DIRECTION ( 'NONE',  ( -0.000000000000000000, -0.000000000000000000, -1.000000000000000000 ) ) ;
#5114 = EDGE_CURVE ( 'NONE', #1714, #26, #8197, .T. ) ;
#5115 = DIRECTION ( 'NONE',  ( 0.000000000000000000, 0.000000000000000000, -1.000000000000000000 ) ) ;
#5116 = ORIENTED_EDGE ( 'NONE', *, *, #726, .T. ) ;
#5117 = CARTESIAN_POINT ( 'NONE',  ( 43.45299461620744808, 50.00000000000000000, -7.500000000000000000 ) ) ;
#5118 = CARTESIAN_POINT ( 'NONE',  ( 4.725907263620340082, -77.40452850542925489, -1.635492904037697981 ) ) ;
#5119 = CARTESIAN_POINT ( 'NONE',  ( 0.09506052544075525856, -76.99547149457073658, -4.999999999999997335 ) ) ;
#5120 = CARTESIAN_POINT ( 'NONE',  ( 2.778853182387016396, -96.99999999999994316, -2.973145269983016092 ) ) ;
#5121 = CARTESIAN_POINT ( 'NONE',  ( 2.823794231030058999, -70.09547149457073090, 1.017458915287723809 ) ) ;
#5122 = CARTESIAN_POINT ( 'NONE',  ( 5.895805022753406455, -80.55452850542926058, -4.407101234057908989 ) ) ;
#5123 = CARTESIAN_POINT ( 'NONE',  ( -4.312004677470992142, -81.04547149457070532, 3.009306630940933758 ) ) ;
#5124 = CARTESIAN_POINT ( 'NONE',  ( 4.312004677471073855, -61.95452850542923784, 3.009306630940844496 ) ) ;
#5125 = CARTESIAN_POINT ( 'NONE',  ( -5.999999999999995559, -27.99999999999999645, -2.499999999999999112 ) ) ;
#5126 = CARTESIAN_POINT ( 'NONE',  ( -6.013306294175152722, -78.45452850542925205, -4.245374608440613429 ) ) ;
#5127 = CARTESIAN_POINT ( 'NONE',  ( 1.686450176301637516, -87.79547149457074795, 2.482926158054096000 ) ) ;
#5128 = ORIENTED_EDGE ( 'NONE', *, *, #2960, .T. ) ;
#5129 = DIRECTION ( 'NONE',  ( 0.000000000000000000, 0.000000000000000000, -1.000000000000000000 ) ) ;
#5130 = DIRECTION ( 'NONE',  ( 0.000000000000000000, 1.000000000000000000, 0.000000000000000000 ) ) ;
#5131 = VERTEX_POINT ( 'NONE', #7975 ) ;
#5132 = CARTESIAN_POINT ( 'NONE',  ( 5.257311121191341030, -77.25452850542926342, -0.09995255151729466603 ) ) ;
#5133 = CARTESIAN_POINT ( 'NONE',  ( 2.610703060766982553, -61.95452850542925916, 1.773238653441072232 ) ) ;
#5134 = CARTESIAN_POINT ( 'NONE',  ( -4.725907263620318766, -93.90452850542925489, 1.635492904037698647 ) ) ;
#5135 = CARTESIAN_POINT ( 'NONE',  ( 4.037591185471561595, -69.79547149457074795, 5.718994135553860936 ) ) ;
#5136 = CARTESIAN_POINT ( 'NONE',  ( -3.015831842038127597, -87.19547149457073942, 3.989209796945492048 ) ) ;
#5137 = CARTESIAN_POINT ( 'NONE',  ( -0.8796985632578796510, -73.35452850542924352, 3.030887037049973198 ) ) ;
#5138 = LINE ( 'NONE', #4006, #4831 ) ;
#5139 = CARTESIAN_POINT ( 'NONE',  ( -5.999999999999993783, -51.00000000000000711, -2.499999999999999112 ) ) ;
#5140 = CARTESIAN_POINT ( 'NONE',  ( -3.154386672714787565, -87.75452850542924921, 0.09995255151727280851 ) ) ;
#5141 = CARTESIAN_POINT ( 'NONE',  ( 7.360235569667875843, -64.24547149457075079, 0.09995255151716216091 ) ) ;
#5142 = EDGE_CURVE ( 'NONE', #549, #1649, #515, .T. ) ;
#5143 = CIRCLE ( 'NONE', #4334, 1.500000000000000666 ) ;
#5144 = CARTESIAN_POINT ( 'NONE',  ( -0.1932469879202498297, -30.15636746936407064, 4.500000000000000888 ) ) ;
#5145 = CARTESIAN_POINT ( 'NONE',  ( -4.194503406049383543, -62.44547149457073232, -3.171033256558012159 ) ) ;
#5146 = CARTESIAN_POINT ( 'NONE',  ( -5.257311121191324155, -59.74547149457072948, -0.09995255151718371311 ) ) ;
#5147 = DIRECTION ( 'NONE',  ( 1.261617073437677752E-16, -1.000000000000000000, -0.000000000000000000 ) ) ;
#5148 = DIRECTION ( 'NONE',  ( 0.000000000000000000, 1.000000000000000000, 0.000000000000000000 ) ) ;
#5149 = EDGE_CURVE ( 'NONE', #914, #5848, #7934, .T. ) ;
#5150 = FILL_AREA_STYLE_COLOUR ( '', #3689 ) ;
#5151 = CARTESIAN_POINT ( 'NONE',  ( 4.037591185471564259, -87.79547149457074795, 5.718994135553860936 ) ) ;
#5152 = ORIENTED_EDGE ( 'NONE', *, *, #2592, .T. ) ;
#5153 = CARTESIAN_POINT ( 'NONE',  ( -1.529537955723670128, -79.35452850542925773, 5.030887037049979860 ) ) ;
#5154 = DIRECTION ( 'NONE',  ( -1.261617073437677752E-16, 1.000000000000000000, 0.000000000000000000 ) ) ;
#5155 = AXIS2_PLACEMENT_3D ( 'NONE', #876, #6565, #7924 ) ;
#5156 = AXIS2_PLACEMENT_3D ( 'NONE', #861, #3441, #6674 ) ;
#5157 = VECTOR ( 'NONE', #1614, 1000.000000000000000 ) ;
#5158 = CARTESIAN_POINT ( 'NONE',  ( 6.123233995736760366E-16, -27.00000000000000000, 5.000000000000000000 ) ) ;
#5159 = AXIS2_PLACEMENT_3D ( 'NONE', #4180, #2923, #6202 ) ;
#5160 = CARTESIAN_POINT ( 'NONE',  ( 4.725907263620372945, -79.09547149457074511, 1.635492904037598283 ) ) ;
#5161 = CARTESIAN_POINT ( 'NONE',  ( 0.000000000000000000, -54.00000000000000711, 0.000000000000000000 ) ) ;
#5162 = CARTESIAN_POINT ( 'NONE',  ( 2.882544866740876177, -67.39547149457074227, -0.8366430509619593447 ) ) ;
#5163 = CARTESIAN_POINT ( 'NONE',  ( -5.895805022753386915, -70.05452850542926058, 4.407101234057909878 ) ) ;
#5164 = LINE ( 'NONE', #7743, #3751 ) ;
#5165 = CARTESIAN_POINT ( 'NONE',  ( 2.862020680886599777, -81.79547149457073374, 4.100960146803977580 ) ) ;
#5166 = CARTESIAN_POINT ( 'NONE',  ( -1.719659006605374962, -57.15452850542924068, -4.969112962950016588 ) ) ;
#5167 = LINE ( 'NONE', #653, #2805 ) ;
#5168 = CARTESIAN_POINT ( 'NONE',  ( 5.895805022753404678, -71.55452850542926058, -4.407101234057908989 ) ) ;
#5169 = VECTOR ( 'NONE', #821, 1000.000000000000000 ) ;
#5170 = CARTESIAN_POINT ( 'NONE',  ( -0.09506052544075668798, -75.49547149457075079, 2.999999999999997780 ) ) ;
#5171 = ORIENTED_EDGE ( 'NONE', *, *, #3794, .T. ) ;
#5172 = DIRECTION ( 'NONE',  ( -1.000000000000000000, 0.000000000000000000, 0.000000000000000000 ) ) ;
#5173 = DIRECTION ( 'NONE',  ( -0.9954714945707483498, -0.09506052544079830746, 1.046913586349167774E-14 ) ) ;
#5174 = CARTESIAN_POINT ( 'NONE',  ( 3.015831842038235955, -91.80452850542926058, 3.989209796945429432 ) ) ;
#5175 = VERTEX_POINT ( 'NONE', #7293 ) ;
#5176 = CARTESIAN_POINT ( 'NONE',  ( 0.09506052544086084077, -82.50452850542926342, 4.999999999999997335 ) ) ;
#5177 = CARTESIAN_POINT ( 'NONE',  ( 1.069819614139555064, -61.65452850542925489, 2.969112962950023249 ) ) ;
#5178 = CARTESIAN_POINT ( 'NONE',  ( 0.000000000000000000, 0.000000000000000000, 0.000000000000000000 ) ) ;
#5179 = CARTESIAN_POINT ( 'NONE',  ( -1.719659006605370744, -87.15452850542926910, -4.969112962950016588 ) ) ;
#5180 = CARTESIAN_POINT ( 'NONE',  ( 4.037591185471560706, -60.79547149457074084, 5.718994135553860936 ) ) ;
#5181 = CLOSED_SHELL ( 'NONE', ( #8149, #4267, #222, #3148, #4460, #2554, #1837, #5537, #6675, #5403, #248, #6391, #7690, #3624, #4138, #6586, #3283, #7847 ) ) ;
#5182 = CARTESIAN_POINT ( 'NONE',  ( -4.784657899331157260, -80.89547149457074227, 1.454677039711874675 ) ) ;
#5183 = CARTESIAN_POINT ( 'NONE',  ( -0.09506052544081895761, -78.00452850542926342, -2.999999999999997780 ) ) ;
#5184 = EDGE_CURVE ( 'NONE', #7308, #3730, #2201, .T. ) ;
#5185 = DIRECTION ( 'NONE',  ( 1.000000000000000000, 0.000000000000000000, -0.000000000000000000 ) ) ;
#5186 = LINE ( 'NONE', #5139, #1754 ) ;
#5187 = CARTESIAN_POINT ( 'NONE',  ( -0.8796985632578775416, -91.35452850542925773, 3.030887037049973198 ) ) ;
#5188 = CARTESIAN_POINT ( 'NONE',  ( -7.360235569667860744, -59.74547149457073658, -0.09995255151716124498 ) ) ;
#5189 = DIRECTION ( 'NONE',  ( -0.000000000000000000, 1.000000000000000000, -0.000000000000000000 ) ) ;
#5190 = CARTESIAN_POINT ( 'NONE',  ( -4.312004677471056979, -81.45452850542923784, -3.009306630940844052 ) ) ;
#5191 = CARTESIAN_POINT ( 'NONE',  ( 6.013306294175080779, -97.54547149457074795, -4.245374608440741326 ) ) ;
#5192 = DIRECTION ( 'NONE',  ( -1.261617073437677752E-16, 1.000000000000000000, 0.000000000000000000 ) ) ;
#5193 = DIRECTION ( 'NONE',  ( 0.000000000000000000, 0.7071067811865507924, 0.7071067811865441310 ) ) ;
#5194 = CARTESIAN_POINT ( 'NONE',  ( -4.312004677471060532, -63.45452850542926626, -3.009306630940844052 ) ) ;
#5195 = CARTESIAN_POINT ( 'NONE',  ( 2.369498399071079842, -94.84547149457073090, -6.969112962950057444 ) ) ;
#5196 = SURFACE_SIDE_STYLE ('',( #6968 ) ) ;
#5197 = ORIENTED_EDGE ( 'NONE', *, *, #3240, .F. ) ;
#5198 = CARTESIAN_POINT ( 'NONE',  ( -4.312004677471057867, -72.45452850542922363, -3.009306630940844052 ) ) ;
#5199 = CARTESIAN_POINT ( 'NONE',  ( -1.500000000000001332, -27.00000000000000000, 2.500000000000000888 ) ) ;
#5200 = FACE_OUTER_BOUND ( 'NONE', #2235, .T. ) ;
#5201 = CARTESIAN_POINT ( 'NONE',  ( -4.194503406049383543, -83.44547149457071100, -3.171033256558012159 ) ) ;
#5202 = DIRECTION ( 'NONE',  ( 0.000000000000000000, 0.7071067811865483499, -0.7071067811865465735 ) ) ;
#5203 = CARTESIAN_POINT ( 'NONE',  ( 1.686450176301634185, -63.79547149457074084, 2.482926158054096000 ) ) ;
#5204 = CARTESIAN_POINT ( 'NONE',  ( -6.628020296210622497, -69.90452850542925489, 2.253526892787613978 ) ) ;
#5205 = CARTESIAN_POINT ( 'NONE',  ( 65.00000000000000000, -12.00000000000000711, 12.49999999999999822 ) ) ;
#5206 = CARTESIAN_POINT ( 'NONE',  ( -1.719659006605265050, -78.34547149457074511, 4.969112962950051227 ) ) ;
#5207 = CARTESIAN_POINT ( 'NONE',  ( -4.312004677471061420, -57.45452850542925916, -3.009306630940844052 ) ) ;
#5208 = CARTESIAN_POINT ( 'NONE',  ( -4.194503406049316041, -85.05452850542926058, 3.171033256558100533 ) ) ;
#5209 = CARTESIAN_POINT ( 'NONE',  ( -4.191402346623180009, -69.30452850542926058, -5.607243785695311900 ) ) ;
#5210 = CARTESIAN_POINT ( 'NONE',  ( 2.610703060766945693, -76.54547149457074795, -1.773238653441125523 ) ) ;
#5211 = AXIS2_PLACEMENT_3D ( 'NONE', #2001, #6460, #4511 ) ;
#5212 = ADVANCED_FACE ( 'NONE', ( #251 ), #4846, .F. ) ;
#5213 = ORIENTED_EDGE ( 'NONE', *, *, #5522, .F. ) ;
#5214 = DIRECTION ( 'NONE',  ( -1.000000000000000000, 0.000000000000000000, 0.000000000000000000 ) ) ;
#5215 = CARTESIAN_POINT ( 'NONE',  ( 80.00000000000000000, -25.00000000000000000, -20.00000000000000000 ) ) ;
#5216 = CARTESIAN_POINT ( 'NONE',  ( 4.312004677471078296, -88.95452850542922363, 3.009306630940844496 ) ) ;
#5217 = ORIENTED_EDGE ( 'NONE', *, *, #359, .T. ) ;
#5218 = CARTESIAN_POINT ( 'NONE',  ( -0.09506052544083921918, -84.00452850542926342, -4.999999999999997335 ) ) ;
#5219 = CARTESIAN_POINT ( 'NONE',  ( -2.882544866740856637, -86.89547149457074227, 0.8366430509619596778 ) ) ;
#5220 = CARTESIAN_POINT ( 'NONE',  ( 0.000000000000000000, 0.000000000000000000, 0.000000000000000000 ) ) ;
#5221 = CARTESIAN_POINT ( 'NONE',  ( -1.529537955723668352, -91.35452850542921510, 5.030887037049979860 ) ) ;
#5222 = CARTESIAN_POINT ( 'NONE',  ( 4.191402346623076980, -61.69547149457074653, -5.607243785695398941 ) ) ;
#5223 = CARTESIAN_POINT ( 'NONE',  ( 1.069819614139555952, -67.65452850542925489, 2.969112962950023249 ) ) ;
#5224 = CARTESIAN_POINT ( 'NONE',  ( -0.9662349396012467340, -27.25766265056033433, 4.500000000000000888 ) ) ;
#5225 = DIRECTION ( 'NONE',  ( 0.000000000000000000, 0.000000000000000000, 1.000000000000000000 ) ) ;
#5226 = CARTESIAN_POINT ( 'NONE',  ( -0.8796985632578782077, -85.35452850542924352, 3.030887037049973198 ) ) ;
#5227 = CARTESIAN_POINT ( 'NONE',  ( 0.09506052544088365586, -94.50452850542926342, 6.999999999999997335 ) ) ;
#5228 = AXIS2_PLACEMENT_3D ( 'NONE', #7072, #7707, #2066 ) ;
#5229 = DIRECTION ( 'NONE',  ( -1.000000000000000000, 0.000000000000000000, 0.000000000000000000 ) ) ;
#5230 = CARTESIAN_POINT ( 'NONE',  ( -5.257311121191324155, -75.75452850542922079, 0.09995255151729526277 ) ) ;
#5231 = CARTESIAN_POINT ( 'NONE',  ( -2.179377348189609265, -92.14547149457074227, -7.030887037049939003 ) ) ;
#5232 = LINE ( 'NONE', #1278, #6297 ) ;
#5233 = DIRECTION ( 'NONE',  ( 0.000000000000000000, 1.000000000000000000, 0.000000000000000000 ) ) ;
#5234 = CARTESIAN_POINT ( 'NONE',  ( -2.493201789345291797, -71.44547149457072521, -1.934965279058240561 ) ) ;
#5235 = AXIS2_PLACEMENT_3D ( 'NONE', #195, #7152, #6556 ) ;
#5236 = CARTESIAN_POINT ( 'NONE',  ( -4.725907263620324095, -57.90452850542925489, 1.635492904037698647 ) ) ;
#5237 = CARTESIAN_POINT ( 'NONE',  ( -2.179377348189609265, -92.14547149457074227, -7.030887037049939003 ) ) ;
#5238 = VERTEX_POINT ( 'NONE', #3498 ) ;
#5239 = CARTESIAN_POINT ( 'NONE',  ( -5.257311121191324155, -75.75452850542922079, 0.09995255151729526277 ) ) ;
#5240 = CARTESIAN_POINT ( 'NONE',  ( 3.943604702053941724E-15, -27.99999999999999645, 2.500000000000000888 ) ) ;
#5241 = CONTEXT_DEPENDENT_SHAPE_REPRESENTATION ( #6154, #5446 ) ;
#5242 = CIRCLE ( 'NONE', #1481, 1.500000000000000666 ) ;
#5243 = DIRECTION ( 'NONE',  ( 0.000000000000000000, 0.000000000000000000, -1.000000000000000000 ) ) ;
#5244 = CARTESIAN_POINT ( 'NONE',  ( 1.529537955723795584, -78.64547149457074227, 5.030887037049945221 ) ) ;
#5245 = CARTESIAN_POINT ( 'NONE',  ( -47.50000000000000711, -49.99999999999998579, -12.50000000000001954 ) ) ;
#5246 = CARTESIAN_POINT ( 'NONE',  ( 2.882544866740875733, -64.39547149457074227, -0.8366430509619593447 ) ) ;
#5247 = CARTESIAN_POINT ( 'NONE',  ( 2.369498399071224171, -67.65452850542925489, 6.969112962950009482 ) ) ;
#5248 = FACE_OUTER_BOUND ( 'NONE', #2567, .T. ) ;
#5249 = ADVANCED_FACE ( 'NONE', ( #1603 ), #5476, .T. ) ;
#5250 = CARTESIAN_POINT ( 'NONE',  ( -0.09506052544073541333, -75.49547149457073658, 4.999999999999997335 ) ) ;
#5251 = CARTESIAN_POINT ( 'NONE',  ( 43.45299461620744097, 100.0000000000000000, 7.500000000000000000 ) ) ;
#5252 = CARTESIAN_POINT ( 'NONE',  ( -0.09506052544083884448, -87.00452850542924921, -4.999999999999997335 ) ) ;
#5253 = COLOUR_RGB ( '', 0.31764706, 0.68627451, 0.89019608) ;
#5254 = CARTESIAN_POINT ( 'NONE',  ( -6.686770931921506289, -69.60452850542924352, -2.072711028461647675 ) ) ;
#5255 = CARTESIAN_POINT ( 'NONE',  ( 2.823794231030059887, -76.09547149457073090, 1.017458915287723809 ) ) ;
#5256 = EDGE_CURVE ( 'NONE', #6564, #3733, #6710, .T. ) ;
#5257 = VERTEX_POINT ( 'NONE', #3706 ) ;
#5258 = DIRECTION ( 'NONE',  ( -0.000000000000000000, 1.000000000000000000, 2.168404344971010347E-16 ) ) ;
#5259 = FACE_OUTER_BOUND ( 'NONE', #3747, .T. ) ;
#5260 = CARTESIAN_POINT ( 'NONE',  ( -1.719659006605370744, -90.15452850542922647, -4.969112962950016588 ) ) ;
#5261 = ORIENTED_EDGE ( 'NONE', *, *, #3472, .T. ) ;
#5262 = CARTESIAN_POINT ( 'NONE',  ( 4.784657899331210551, -80.10452850542925773, 1.454677039711774533 ) ) ;
#5263 = CARTESIAN_POINT ( 'NONE',  ( -1.686450176301614867, -92.29547149457074795, -2.482926158054096000 ) ) ;
#5264 = DIRECTION ( 'NONE',  ( 1.000000000000000000, 0.000000000000000000, 0.000000000000000000 ) ) ;
#5265 = CARTESIAN_POINT ( 'NONE',  ( -5.257311121191323267, -84.75452850542923500, 0.09995255151729526277 ) ) ;
#5266 = EDGE_CURVE ( 'NONE', #348, #2974, #3486, .T. ) ;
#5267 = CARTESIAN_POINT ( 'NONE',  ( 0.09506052544088365586, -94.50452850542926342, 6.999999999999997335 ) ) ;
#5268 = CARTESIAN_POINT ( 'NONE',  ( -1.069819614139540187, -63.15452850542925489, -2.969112962950023249 ) ) ;
#5269 = PLANE ( 'NONE',  #5908 ) ;
#5270 = CYLINDRICAL_SURFACE ( 'NONE', #7267, 5.000000000000000888 ) ;
#5271 = CARTESIAN_POINT ( 'NONE',  ( 2.823794231030040791, -80.40452850542925489, -1.017458915287783316 ) ) ;
#5272 = CARTESIAN_POINT ( 'NONE',  ( -6.013306294175149169, -90.45452850542926626, -4.245374608440613429 ) ) ;
#5273 = DIRECTION ( 'NONE',  ( -0.000000000000000000, -0.000000000000000000, -1.000000000000000000 ) ) ;
#5274 = CARTESIAN_POINT ( 'NONE',  ( 5.895805022753496161, -84.94547149457073942, 4.407101234057782868 ) ) ;
#5275 = DIRECTION ( 'NONE',  ( 1.261617073437677752E-16, -1.000000000000000000, -0.000000000000000000 ) ) ;
#5276 = CYLINDRICAL_SURFACE ( 'NONE', #6626, 5.000000000000004441 ) ;
#5277 = CARTESIAN_POINT ( 'NONE',  ( 2.493201789345308672, -66.94547149457073942, 1.934965279058241006 ) ) ;
#5278 = CARTESIAN_POINT ( 'NONE',  ( -5.257311121191324155, -57.75452850542923500, 0.09995255151729526277 ) ) ;
#5279 = ORIENTED_EDGE ( 'NONE', *, *, #3240, .T. ) ;
#5280 = CARTESIAN_POINT ( 'NONE',  ( -3.015831842038216859, -63.30452850542925347, -3.989209796945429432 ) ) ;
#5281 = CARTESIAN_POINT ( 'NONE',  ( 6.013306294175080779, -85.54547149457074795, -4.245374608440741326 ) ) ;
#5282 = ORIENTED_EDGE ( 'NONE', *, *, #1098, .T. ) ;
#5283 = CARTESIAN_POINT ( 'NONE',  ( 5.257311121191341918, -77.25452850542926342, -0.09995255151729465215 ) ) ;
#5284 = ADVANCED_FACE ( 'NONE', ( #2443 ), #6232, .F. ) ;
#5285 = DIRECTION ( 'NONE',  ( 1.000000000000000000, 0.000000000000000000, -0.000000000000000000 ) ) ;
#5286 = LINE ( 'NONE', #3983, #2080 ) ;
#5287 = CARTESIAN_POINT ( 'NONE',  ( 4.194503406049402194, -75.94547149457075363, 3.171033256558012159 ) ) ;
#5288 = CARTESIAN_POINT ( 'NONE',  ( 50.00000000000000000, -1.734723475976807094E-15, 12.50000000000000000 ) ) ;
#5289 = CARTESIAN_POINT ( 'NONE',  ( 2.493201789345307784, -60.94547149457074653, 1.934965279058241006 ) ) ;
#5290 = CARTESIAN_POINT ( 'NONE',  ( 4.037591185471441690, -71.70452850542925205, -5.718994135553947977 ) ) ;
#5291 = DIRECTION ( 'NONE',  ( 0.000000000000000000, 0.000000000000000000, 1.000000000000000000 ) ) ;
#5292 = CARTESIAN_POINT ( 'NONE',  ( -1.529537955723776710, -80.14547149457072805, -5.030887037049945221 ) ) ;
#5293 =( REPRESENTATION_RELATIONSHIP ('NONE','NONE', #4188, #1613 ) REPRESENTATION_RELATIONSHIP_WITH_TRANSFORMATION ( #3314 )SHAPE_REPRESENTATION_RELATIONSHIP( ) );
#5294 = PLANE ( 'NONE',  #7881 ) ;
#5295 = CARTESIAN_POINT ( 'NONE',  ( 5.257311121191342806, -89.25452850542924921, -0.09995255151729465215 ) ) ;
#5296 = CARTESIAN_POINT ( 'NONE',  ( -2.369498399071207739, -72.15452850542922647, -6.969112962950009482 ) ) ;
#5297 = CARTESIAN_POINT ( 'NONE',  ( -1.686450176301616866, -77.29547149457074795, -2.482926158054096000 ) ) ;
#5298 = AXIS2_PLACEMENT_3D ( 'NONE', #7550, #6243, #4337 ) ;
#5299 = AXIS2_PLACEMENT_3D ( 'NONE', #6886, #525, #1679 ) ;
#5300 = EDGE_LOOP ( 'NONE', ( #4532, #5349, #2376, #3851 ) ) ;
#5301 = DIRECTION ( 'NONE',  ( 0.000000000000000000, -2.168404344971010101E-16, 1.000000000000000000 ) ) ;
#5302 = CARTESIAN_POINT ( 'NONE',  ( -4.784657899331188347, -93.60452850542925773, -1.454677039711773867 ) ) ;
#5303 = CARTESIAN_POINT ( 'NONE',  ( -1.529537955723668352, -91.35452850542921510, 5.030887037049979860 ) ) ;
#5304 = ORIENTED_EDGE ( 'NONE', *, *, #5575, .T. ) ;
#5305 = CARTESIAN_POINT ( 'NONE',  ( 4.725907263620340082, -77.40452850542925489, -1.635492904037697981 ) ) ;
#5306 = CARTESIAN_POINT ( 'NONE',  ( -2.610703060766923933, -90.04547149457074795, 1.773238653441125745 ) ) ;
#5307 = AXIS2_PLACEMENT_3D ( 'NONE', #5240, #7952, #4602 ) ;
#5308 = CARTESIAN_POINT ( 'NONE',  ( -4.725907263620319654, -87.90452850542926910, 1.635492904037698647 ) ) ;
#5309 = CARTESIAN_POINT ( 'NONE',  ( 6.013306294175172262, -94.95452850542926626, 4.245374608440616093 ) ) ;
#5310 = CARTESIAN_POINT ( 'NONE',  ( 2.493201789345269592, -62.55452850542925347, -1.934965279058294518 ) ) ;
#5311 = PLANE ( 'NONE',  #3079 ) ;
#5312 = FACE_OUTER_BOUND ( 'NONE', #4104, .T. ) ;
#5313 = CARTESIAN_POINT ( 'NONE',  ( -2.823794231030020363, -81.90452850542925489, 1.017458915287783316 ) ) ;
#5314 = CARTESIAN_POINT ( 'NONE',  ( -4.191402346623176456, -93.30452850542926058, -5.607243785695311900 ) ) ;
#5315 = CLOSED_SHELL ( 'NONE', ( #2856, #6616, #4499, #4108, #4660, #5872, #1721, #635, #6612, #4786, #2760, #1913, #5347 ) ) ;
#5316 = DIRECTION ( 'NONE',  ( 0.000000000000000000, 0.000000000000000000, 1.000000000000000000 ) ) ;
#5317 = CARTESIAN_POINT ( 'NONE',  ( -7.360235569667856304, -89.74547149457073658, -0.09995255151716124498 ) ) ;
#5318 = CARTESIAN_POINT ( 'NONE',  ( -80.00100000000001899, -88.00000000000004263, 0.000000000000000000 ) ) ;
#5319 = CARTESIAN_POINT ( 'NONE',  ( 1.500000000000002665, -27.00000000000000000, 2.500000000000000888 ) ) ;
#5320 = CARTESIAN_POINT ( 'NONE',  ( -3.154386672714791118, -65.74547149457073658, -0.09995255151720625064 ) ) ;
#5321 = ORIENTED_EDGE ( 'NONE', *, *, #1981, .F. ) ;
#5322 = EDGE_CURVE ( 'NONE', #604, #4154, #6276, .T. ) ;
#5323 = CARTESIAN_POINT ( 'NONE',  ( -4.312004677471057867, -72.45452850542922363, -3.009306630940844052 ) ) ;
#5324 = CARTESIAN_POINT ( 'NONE',  ( -2.179377348189610597, -80.14547149457074227, -7.030887037049939003 ) ) ;
#5325 = SURFACE_STYLE_USAGE ( .BOTH. , #4646 ) ;
#5326 = EDGE_CURVE ( 'NONE', #2522, #2431, #494, .T. ) ;
#5327 = ORIENTED_EDGE ( 'NONE', *, *, #6707, .T. ) ;
#5328 = CARTESIAN_POINT ( 'NONE',  ( 4.725907263620340082, -71.40452850542925489, -1.635492904037697981 ) ) ;
#5329 = LINE ( 'NONE', #145, #7054 ) ;
#5330 = CARTESIAN_POINT ( 'NONE',  ( 3.015831842038148469, -73.69547149457073942, -3.989209796945492048 ) ) ;
#5331 = DIRECTION ( 'NONE',  ( 0.000000000000000000, -1.000000000000000000, 0.000000000000000000 ) ) ;
#5332 = CARTESIAN_POINT ( 'NONE',  ( -2.610703060766927042, -66.04547149457074795, 1.773238653441125745 ) ) ;
#5333 = CARTESIAN_POINT ( 'NONE',  ( -6.686770931921506289, -69.60452850542924352, -2.072711028461647675 ) ) ;
#5334 = LINE ( 'NONE', #5205, #3086 ) ;
#5335 = CARTESIAN_POINT ( 'NONE',  ( -4.784657899331190123, -84.60452850542927195, -1.454677039711773867 ) ) ;
#5336 = CARTESIAN_POINT ( 'NONE',  ( 5.895805022753404678, -68.55452850542926058, -4.407101234057908989 ) ) ;
#5337 = CARTESIAN_POINT ( 'NONE',  ( 2.823794231030060331, -82.09547149457075932, 1.017458915287723809 ) ) ;
#5338 = ORIENTED_EDGE ( 'NONE', *, *, #1320, .F. ) ;
#5339 = CARTESIAN_POINT ( 'NONE',  ( 45.00000000000000000, -14.99999999999999467, -12.50000000000000178 ) ) ;
#5340 = CARTESIAN_POINT ( 'NONE',  ( -4.312004677471055203, -93.45452850542922363, -3.009306630940844052 ) ) ;
#5341 = CARTESIAN_POINT ( 'NONE',  ( 4.194503406049338246, -80.55452850542926058, -3.171033256558100089 ) ) ;
#5342 = ORIENTED_EDGE ( 'NONE', *, *, #4118, .F. ) ;
#5343 = CARTESIAN_POINT ( 'NONE',  ( 0.09506052544085932809, -70.50452850542926342, 4.999999999999997335 ) ) ;
#5344 = CARTESIAN_POINT ( 'NONE',  ( -1.069819614139473352, -87.34547149457073090, 2.969112962950044121 ) ) ;
#5345 = CARTESIAN_POINT ( 'NONE',  ( -0.09506052544083846978, -90.00452850542924921, -4.999999999999997335 ) ) ;
#5346 = CARTESIAN_POINT ( 'NONE',  ( -4.037591185471420374, -94.20452850542928047, 5.718994135553947977 ) ) ;
#5347 = ADVANCED_FACE ( 'NONE', ( #3623 ), #7501, .F. ) ;
#5348 = CARTESIAN_POINT ( 'NONE',  ( 2.610703060766982553, -61.95452850542925916, 1.773238653441072232 ) ) ;
#5349 = ORIENTED_EDGE ( 'NONE', *, *, #3407, .F. ) ;
#5350 = DIRECTION ( 'NONE',  ( 1.000000000000000000, 0.000000000000000000, 0.000000000000000000 ) ) ;
#5351 = CIRCLE ( 'NONE', #7645, 4.999999999999999112 ) ;
#5352 = CARTESIAN_POINT ( 'NONE',  ( 63.45299461620744808, 100.0000000000000000, -7.500000000000000000 ) ) ;
#5353 = CARTESIAN_POINT ( 'NONE',  ( -0.8796985632578793179, -76.35452850542924352, 3.030887037049973198 ) ) ;
#5354 = CARTESIAN_POINT ( 'NONE',  ( 6.628020296210642037, -92.40452850542925489, -2.253526892787612645 ) ) ;
#5355 = CARTESIAN_POINT ( 'NONE',  ( 5.895805022753496161, -90.94547149457073942, 4.407101234057782868 ) ) ;
#5356 = CARTESIAN_POINT ( 'NONE',  ( 43.45299461620744808, 50.00000000000000000, 7.500000000000000000 ) ) ;
#5357 = PRODUCT_DEFINITION ( 'UNKNOWN', '', #7127, #4768 ) ;
#5358 = DIRECTION ( 'NONE',  ( 0.000000000000000000, -0.7071067811865507924, 0.7071067811865441310 ) ) ;
#5359 = CARTESIAN_POINT ( 'NONE',  ( 2.882544866740876177, -67.39547149457074227, -0.8366430509619593447 ) ) ;
#5360 = PRODUCT_DEFINITION_CONTEXT ( 'detailed design', #6318, 'design' ) ;
#5361 = CARTESIAN_POINT ( 'NONE',  ( -55.00000000000000000, -25.00000000000002132, -20.00000000000000000 ) ) ;
#5362 = ORIENTED_EDGE ( 'NONE', *, *, #3325, .F. ) ;
#5363 = CARTESIAN_POINT ( 'NONE',  ( 1.719659006605389617, -67.65452850542925489, 4.969112962950016588 ) ) ;
#5364 = CARTESIAN_POINT ( 'NONE',  ( 6.013306294175080779, -82.54547149457074795, -4.245374608440741326 ) ) ;
#5365 = EDGE_LOOP ( 'NONE', ( #5197, #6528, #5670, #8237 ) ) ;
#5366 = CARTESIAN_POINT ( 'NONE',  ( -0.09506052544084148126, -66.00452850542926342, -4.999999999999997335 ) ) ;
#5367 = CARTESIAN_POINT ( 'NONE',  ( -1.739222891282244055, -24.35895783175659446, 4.500000000000000888 ) ) ;
#5368 = CIRCLE ( 'NONE', #115, 1.499999999999999556 ) ;
#5369 = PRODUCT_DEFINITION_FORMATION_WITH_SPECIFIED_SOURCE ( 'ANY', '', #8042, .NOT_KNOWN. ) ;
#5370 = CARTESIAN_POINT ( 'NONE',  ( 4.725907263620372056, -67.09547149457073090, 1.635492904037598283 ) ) ;
#5371 = DIRECTION ( 'NONE',  ( 0.000000000000000000, -1.000000000000000000, 0.000000000000000000 ) ) ;
#5372 = CARTESIAN_POINT ( 'NONE',  ( -1.840261337453202195, -63.19547149457074653, 2.371175808195584267 ) ) ;
#5373 = CARTESIAN_POINT ( 'NONE',  ( -2.179377348189463159, -64.35452850542924352, 7.030887037049988741 ) ) ;
#5374 = VERTEX_POINT ( 'NONE', #7462 ) ;
#5375 = EDGE_CURVE ( 'NONE', #1819, #3497, #1732, .T. ) ;
#5376 = DIRECTION ( 'NONE',  ( -0.5000000000000011102, 0.8660254037844380415, 0.000000000000000000 ) ) ;
#5377 = CARTESIAN_POINT ( 'NONE',  ( -5.257311121191322378, -87.75452850542922079, 0.09995255151729526277 ) ) ;
#5378 = CARTESIAN_POINT ( 'NONE',  ( -6.013306294175153610, -63.45452850542924494, -4.245374608440613429 ) ) ;
#5379 = ADVANCED_FACE ( 'NONE', ( #1692 ), #6819, .F. ) ;
#5380 = CIRCLE ( 'NONE', #7672, 1.499999999999996225 ) ;
#5381 = CARTESIAN_POINT ( 'NONE',  ( 2.823794231030059443, -73.09547149457071669, 1.017458915287723809 ) ) ;
#5382 = VERTEX_POINT ( 'NONE', #7578 ) ;
#5383 = CARTESIAN_POINT ( 'NONE',  ( 1.500000000000002442, -27.00000000000000000, 5.000000000000000000 ) ) ;
#5384 = CARTESIAN_POINT ( 'NONE',  ( 4.194503406049339134, -92.55452850542924637, -3.171033256558100089 ) ) ;
#5385 = CARTESIAN_POINT ( 'NONE',  ( 0.09506052544086007750, -76.50452850542924921, 4.999999999999997335 ) ) ;
#5386 = VERTEX_POINT ( 'NONE', #5048 ) ;
#5387 = CARTESIAN_POINT ( 'NONE',  ( 4.194503406049336469, -71.55452850542926058, -3.171033256558100977 ) ) ;
#5388 = CARTESIAN_POINT ( 'NONE',  ( 2.493201789345311781, -93.94547149457073942, 1.934965279058241006 ) ) ;
#5389 = CARTESIAN_POINT ( 'NONE',  ( -2.862020680886578461, -95.29547149457074795, -4.100960146803977580 ) ) ;
#5390 = CARTESIAN_POINT ( 'NONE',  ( 3.015831842038233734, -76.80452850542926058, 3.989209796945429432 ) ) ;
#5391 = CARTESIAN_POINT ( 'NONE',  ( -4.191402346623177344, -90.30452850542926058, -5.607243785695311900 ) ) ;
#5392 = CARTESIAN_POINT ( 'NONE',  ( 2.882544866740895717, -71.10452850542924352, 0.8366430509618999478 ) ) ;
#5393 = ORIENTED_EDGE ( 'NONE', *, *, #5184, .T. ) ;
#5394 = CARTESIAN_POINT ( 'NONE',  ( 80.00000000000000000, -12.00000000000000711, 12.49999999999999822 ) ) ;
#5395 = CARTESIAN_POINT ( 'NONE',  ( 75.00000000000000000, -30.00000000000000000, -7.500000000000007105 ) ) ;
#5396 = CARTESIAN_POINT ( 'NONE',  ( -3.154386672714789785, -75.75452850542926342, 0.09995255151727280851 ) ) ;
#5397 = CARTESIAN_POINT ( 'NONE',  ( 0.09506052544088250400, -85.50452850542926342, 6.999999999999997335 ) ) ;
#5398 = CARTESIAN_POINT ( 'NONE',  ( 6.628020296210689111, -88.09547149457074511, 2.253526892787472757 ) ) ;
#5399 = CARTESIAN_POINT ( 'NONE',  ( 47.49999999999999289, -198.2344135219424857, 12.49999999999993960 ) ) ;
#5400 = LINE ( 'NONE', #7981, #5157 ) ;
#5401 = CARTESIAN_POINT ( 'NONE',  ( 2.882544866740875733, -64.39547149457074227, -0.8366430509619593447 ) ) ;
#5402 = ORIENTED_EDGE ( 'NONE', *, *, #5463, .F. ) ;
#5403 = ADVANCED_FACE ( 'NONE', ( #2950 ), #1771, .T. ) ;
#5404 = CARTESIAN_POINT ( 'NONE',  ( -0.09506052544084073186, -72.00452850542926342, -4.999999999999997335 ) ) ;
#5405 = CARTESIAN_POINT ( 'NONE',  ( -0.09506052544071341703, -81.49547149457075079, 6.999999999999997335 ) ) ;
#5406 = SURFACE_STYLE_FILL_AREA ( #265 ) ;
#5407 = DIRECTION ( 'NONE',  ( 1.000000000000000000, 0.000000000000000000, 0.000000000000000000 ) ) ;
#5408 = PRODUCT_DEFINITION_SHAPE ( 'NONE', 'NONE',  #2017 ) ;
#5409 = CARTESIAN_POINT ( 'NONE',  ( -4.784657899331158148, -77.89547149457074227, 1.454677039711874675 ) ) ;
#5410 = CARTESIAN_POINT ( 'NONE',  ( 0.09506052544085895339, -67.50452850542926342, 4.999999999999997335 ) ) ;
#5411 = CARTESIAN_POINT ( 'NONE',  ( -65.00000000000000000, -7.999999999999992895, -12.50000000000000178 ) ) ;
#5412 = EDGE_CURVE ( 'NONE', #5453, #970, #5593, .T. ) ;
#5413 = CARTESIAN_POINT ( 'NONE',  ( -4.312004677470994807, -66.04547149457074795, 3.009306630940933758 ) ) ;
#5414 = LINE ( 'NONE', #231, #2426 ) ;
#5415 = CARTESIAN_POINT ( 'NONE',  ( -4.725907263620350740, -95.59547149457074511, -1.635492904037597617 ) ) ;
#5416 = CARTESIAN_POINT ( 'NONE',  ( 7.360235569667875843, -59.25452850542926342, -0.09995255151731691212 ) ) ;
#5417 = ORIENTED_EDGE ( 'NONE', *, *, #4590, .F. ) ;
#5418 = AXIS2_PLACEMENT_3D ( 'NONE', #3307, #7221, #4552 ) ;
#5419 =( LENGTH_UNIT ( ) NAMED_UNIT ( * ) SI_UNIT ( .MILLI., .METRE. ) );
#5420 = CARTESIAN_POINT ( 'NONE',  ( 4.194503406049338246, -80.55452850542926058, -3.171033256558100089 ) ) ;
#5421 = ORIENTED_EDGE ( 'NONE', *, *, #6256, .F. ) ;
#5422 = LINE ( 'NONE', #833, #7450 ) ;
#5423 = CARTESIAN_POINT ( 'NONE',  ( -2.862020680886493196, -85.20452850542925205, 4.100960146804039752 ) ) ;
#5424 = CARTESIAN_POINT ( 'NONE',  ( -5.257311121191324155, -75.75452850542922079, 0.09995255151729526277 ) ) ;
#5425 = ORIENTED_EDGE ( 'NONE', *, *, #3107, .F. ) ;
#5426 = CARTESIAN_POINT ( 'NONE',  ( -1.719659006605372964, -72.15452850542924068, -4.969112962950015699 ) ) ;
#5427 = CARTESIAN_POINT ( 'NONE',  ( -1.840261337453199531, -84.19547149457073942, 2.371175808195584267 ) ) ;
#5428 = CARTESIAN_POINT ( 'NONE',  ( 0.09506052544075790922, -97.99547149457075079, -4.999999999999997335 ) ) ;
#5429 = EDGE_CURVE ( 'NONE', #2862, #184, #1177, .T. ) ;
#5430 = CARTESIAN_POINT ( 'NONE',  ( -4.725907263620321430, -75.90452850542925489, 1.635492904037698647 ) ) ;
#5431 = CARTESIAN_POINT ( 'NONE',  ( -7.360235569667858080, -84.75452850542926342, 0.09995255151731782806 ) ) ;
#5432 = AXIS2_PLACEMENT_3D ( 'NONE', #1221, #539, #7668 ) ;
#5433 = VECTOR ( 'NONE', #1000, 1000.000000000000000 ) ;
#5434 = CARTESIAN_POINT ( 'NONE',  ( 0.8796985632579643610, -96.64547149457075648, 3.030887037049952326 ) ) ;
#5435 = ORIENTED_EDGE ( 'NONE', *, *, #353, .T. ) ;
#5436 = CARTESIAN_POINT ( 'NONE',  ( 45.00000000000000000, -14.99999999999999467, 9.499999999999996447 ) ) ;
#5437 = AXIS2_PLACEMENT_3D ( 'NONE', #6839, #434, #3008 ) ;
#5438 = DIRECTION ( 'NONE',  ( 1.000000000000000000, 0.000000000000000000, 0.000000000000000000 ) ) ;
#5439 = CARTESIAN_POINT ( 'NONE',  ( 3.154386672714808437, -74.25452850542924921, -0.09995255151727241993 ) ) ;
#5440 = CARTESIAN_POINT ( 'NONE',  ( -6.628020296210620721, -84.90452850542926910, 2.253526892787613978 ) ) ;
#5441 = CARTESIAN_POINT ( 'NONE',  ( -7.360235569667858080, -83.74547149457075079, -0.09995255151716124498 ) ) ;
#5442 = EDGE_CURVE ( 'NONE', #1841, #5112, #456, .T. ) ;
#5443 = DIRECTION ( 'NONE',  ( 0.000000000000000000, 1.000000000000000000, 2.168404344971010347E-16 ) ) ;
#5444 = DIRECTION ( 'NONE',  ( 0.000000000000000000, -1.000000000000000000, 0.000000000000000000 ) ) ;
#5445 = CARTESIAN_POINT ( 'NONE',  ( -3.154386672714789341, -81.75452850542926342, 0.09995255151727280851 ) ) ;
#5446 = PRODUCT_DEFINITION_SHAPE ( 'NONE', 'NONE',  #8348 ) ;
#5447 = UNCERTAINTY_MEASURE_WITH_UNIT (LENGTH_MEASURE( 1.000000000000000082E-05 ), #2380, 'distance_accuracy_value', 'NONE');
#5448 = DIRECTION ( 'NONE',  ( 1.000000000000000000, 9.251858538542971581E-17, 0.000000000000000000 ) ) ;
#5449 = VERTEX_POINT ( 'NONE', #538 ) ;
#5450 = CARTESIAN_POINT ( 'NONE',  ( 50.00000000000000000, -12.00000000000000355, -12.50000000000000178 ) ) ;
#5451 = CARTESIAN_POINT ( 'NONE',  ( -2.862020680886495860, -64.20452850542926626, 4.100960146804039752 ) ) ;
#5452 = CARTESIAN_POINT ( 'NONE',  ( 2.179377348189630137, -81.64547149457074227, 7.030887037049939003 ) ) ;
#5453 = VERTEX_POINT ( 'NONE', #416 ) ;
#5454 = CARTESIAN_POINT ( 'NONE',  ( 0.09506052544075488386, -73.99547149457075079, -4.999999999999997335 ) ) ;
#5455 = CARTESIAN_POINT ( 'NONE',  ( -4.784657899331159925, -65.89547149457074227, 1.454677039711874675 ) ) ;
#5456 = CARTESIAN_POINT ( 'NONE',  ( -4.784657899331191899, -63.60452850542925063, -1.454677039711773867 ) ) ;
#5457 = CYLINDRICAL_SURFACE ( 'NONE', #8000, 1.500000000000000666 ) ;
#5458 = EDGE_CURVE ( 'NONE', #2526, #6097, #2989, .T. ) ;
#5459 = CARTESIAN_POINT ( 'NONE',  ( -1.719659006605266827, -69.34547149457074511, 4.969112962950051227 ) ) ;
#5460 = CARTESIAN_POINT ( 'NONE',  ( 6.628020296210639373, -62.40452850542925489, -2.253526892787612645 ) ) ;
#5461 = VERTEX_POINT ( 'NONE', #2324 ) ;
#5462 = CYLINDRICAL_SURFACE ( 'NONE', #4099, 1.500000000000001332 ) ;
#5463 = EDGE_CURVE ( 'NONE', #4811, #4198, #5368, .T. ) ;
#5464 = ORIENTED_EDGE ( 'NONE', *, *, #527, .F. ) ;
#5465 = CARTESIAN_POINT ( 'NONE',  ( 80.00000000000000000, -12.00000000000000355, -12.50000000000000178 ) ) ;
#5466 = CARTESIAN_POINT ( 'NONE',  ( 1.529537955723691889, -86.85452850542921510, -5.030887037049978971 ) ) ;
#5467 = CARTESIAN_POINT ( 'NONE',  ( -4.725907263620320542, -78.90452850542925489, 1.635492904037698647 ) ) ;
#5468 = ORIENTED_EDGE ( 'NONE', *, *, #7757, .F. ) ;
#5469 = CARTESIAN_POINT ( 'NONE',  ( -1.529537955723671683, -67.35452850542925773, 5.030887037049979860 ) ) ;
#5470 = CARTESIAN_POINT ( 'NONE',  ( 2.882544866740877954, -82.39547149457074227, -0.8366430509619593447 ) ) ;
#5471 = CARTESIAN_POINT ( 'NONE',  ( -2.823794231030042123, -62.59547149457074511, -1.017458915287723364 ) ) ;
#5472 = CARTESIAN_POINT ( 'NONE',  ( 1.719659006605390283, -73.65452850542924068, 4.969112962950016588 ) ) ;
#5473 = CARTESIAN_POINT ( 'NONE',  ( -2.369498399071205963, -84.15452850542925489, -6.969112962950009482 ) ) ;
#5474 = CARTESIAN_POINT ( 'NONE',  ( 3.154386672714811990, -97.24547149457075079, 0.09995255151720662534 ) ) ;
#5475 = ORIENTED_EDGE ( 'NONE', *, *, #4189, .T. ) ;
#5476 = PLANE ( 'NONE',  #7938 ) ;
#5477 = PRODUCT_DEFINITION_SHAPE ( 'NONE', 'NONE',  #8339 ) ;
#5478 = ORIENTED_EDGE ( 'NONE', *, *, #1489, .T. ) ;
#5479 = CARTESIAN_POINT ( 'NONE',  ( -1.739222891282244055, -24.35895783175659446, 4.500000000000000888 ) ) ;
#5480 = CARTESIAN_POINT ( 'NONE',  ( 0.8796985632578979697, -68.85452850542924352, -3.030887037049972310 ) ) ;
#5481 = CARTESIAN_POINT ( 'NONE',  ( -6.628020296210667794, -77.59547149457073090, -2.253526892787471869 ) ) ;
#5482 = CARTESIAN_POINT ( 'NONE',  ( 80.00000000000000000, -1.734723475976807094E-15, 12.50000000000000000 ) ) ;
#5483 = CARTESIAN_POINT ( 'NONE',  ( -4.312004677470991254, -93.04547149457074795, 3.009306630940933314 ) ) ;
#5484 = CARTESIAN_POINT ( 'NONE',  ( -2.493201789345251385, -82.05452850542926058, 1.934965279058294518 ) ) ;
#5485 = VECTOR ( 'NONE', #2564, 1000.000000000000000 ) ;
#5486 = LINE ( 'NONE', #4217, #2753 ) ;
#5487 = EDGE_LOOP ( 'NONE', ( #5867, #4381 ) ) ;
#5488 = DIRECTION ( 'NONE',  ( 1.000000000000000000, 0.000000000000000000, 0.000000000000000000 ) ) ;
#5489 = CARTESIAN_POINT ( 'NONE',  ( -3.015831842038216859, -60.30452850542926058, -3.989209796945429432 ) ) ;
#5490 = CARTESIAN_POINT ( 'NONE',  ( 5.895805022753492608, -66.94547149457073942, 4.407101234057782868 ) ) ;
#5491 = ORIENTED_EDGE ( 'NONE', *, *, #843, .F. ) ;
#5492 = CARTESIAN_POINT ( 'NONE',  ( -3.015831842038129817, -72.19547149457073942, 3.989209796945492048 ) ) ;
#5493 = CARTESIAN_POINT ( 'NONE',  ( 4.725907263620372056, -70.09547149457074511, 1.635492904037598283 ) ) ;
#5494 = CARTESIAN_POINT ( 'NONE',  ( 0.09506052544085819012, -61.50452850542925631, 4.999999999999997335 ) ) ;
#5495 = FACE_BOUND ( 'NONE', #7580, .T. ) ;
#5496 = CARTESIAN_POINT ( 'NONE',  ( 5.257311121191341918, -67.24547149457075079, 0.09995255151718437925 ) ) ;
#5497 = DIRECTION ( 'NONE',  ( 0.000000000000000000, 0.000000000000000000, 1.000000000000000000 ) ) ;
#5498 = CARTESIAN_POINT ( 'NONE',  ( 0.09506052544087949252, -61.50452850542925631, 6.999999999999997335 ) ) ;
#5499 = VERTEX_POINT ( 'NONE', #3116 ) ;
#5500 = VECTOR ( 'NONE', #4406, 1000.000000000000000 ) ;
#5501 = FACE_OUTER_BOUND ( 'NONE', #875, .T. ) ;
#5502 = AXIS2_PLACEMENT_3D ( 'NONE', #3248, #6531, #5264 ) ;
#5503 = VERTEX_POINT ( 'NONE', #373 ) ;
#5504 = COLOUR_RGB ( '', 0.08235294, 0.09019608, 0.10196078) ;
#5505 = CARTESIAN_POINT ( 'NONE',  ( 80.00000000000000000, 0.000000000000000000, 20.00000000000000000 ) ) ;
#5506 = CARTESIAN_POINT ( 'NONE',  ( 1.719659006605392504, -88.65452850542925489, 4.969112962950016588 ) ) ;
#5507 = CARTESIAN_POINT ( 'NONE',  ( -2.862020680886494084, -79.20452850542925205, 4.100960146804039752 ) ) ;
#5508 = CARTESIAN_POINT ( 'NONE',  ( -3.015831842038216859, -60.30452850542926058, -3.989209796945429432 ) ) ;
#5509 = CARTESIAN_POINT ( 'NONE',  ( -2.493201789345290464, -77.44547149457073942, -1.934965279058240561 ) ) ;
#5510 = CARTESIAN_POINT ( 'NONE',  ( -1.719659006605263496, -96.34547149457074511, 4.969112962950051227 ) ) ;
#5511 = CARTESIAN_POINT ( 'NONE',  ( 4.784657899331208775, -68.10452850542925773, 1.454677039711774533 ) ) ;
#5512 = AXIS2_PLACEMENT_3D ( 'NONE', #8101, #4090, #1694 ) ;
#5513 = CARTESIAN_POINT ( 'NONE',  ( -5.895805022753386027, -85.05452850542926058, 4.407101234057909878 ) ) ;
#5514 = CARTESIAN_POINT ( 'NONE',  ( 0.09506052544077894795, -97.99547149457075079, -2.999999999999997780 ) ) ;
#5515 = EDGE_CURVE ( 'NONE', #7308, #2526, #6900, .T. ) ;
#5516 = PRODUCT_CONTEXT ( 'NONE', #7773, 'mechanical' ) ;
#5517 = ORIENTED_EDGE ( 'NONE', *, *, #5375, .F. ) ;
#5518 = CARTESIAN_POINT ( 'NONE',  ( 43.45299461620743386, 65.00000000000000000, 7.500000000000000000 ) ) ;
#5519 = VERTEX_POINT ( 'NONE', #5518 ) ;
#5520 = CARTESIAN_POINT ( 'NONE',  ( 65.00000000000000000, -12.00000000000000711, 12.49999999999999822 ) ) ;
#5521 = CARTESIAN_POINT ( 'NONE',  ( 2.493201789345271369, -71.55452850542926058, -1.934965279058294518 ) ) ;
#5522 = EDGE_CURVE ( 'NONE', #731, #7486, #5556, .T. ) ;
#5523 = CARTESIAN_POINT ( 'NONE',  ( -4.191402346623057440, -81.19547149457073942, 5.607243785695398941 ) ) ;
#5524 = CARTESIAN_POINT ( 'NONE',  ( -5.257311121191322378, -90.75452850542924921, 0.09995255151729526277 ) ) ;
#5525 = CARTESIAN_POINT ( 'NONE',  ( 1.529537955723798248, -96.64547149457072805, 5.030887037049945221 ) ) ;
#5526 = CARTESIAN_POINT ( 'NONE',  ( -1.069819614139537967, -81.15452850542924068, -2.969112962950023249 ) ) ;
#5527 = ORIENTED_EDGE ( 'NONE', *, *, #2485, .F. ) ;
#5528 = FACE_OUTER_BOUND ( 'NONE', #1062, .T. ) ;
#5529 = CARTESIAN_POINT ( 'NONE',  ( -2.862020680886496304, -61.20452850542925205, 4.100960146804039752 ) ) ;
#5530 = CARTESIAN_POINT ( 'NONE',  ( -6.628020296210667794, -74.59547149457071669, -2.253526892787471869 ) ) ;
#5531 = ORIENTED_EDGE ( 'NONE', *, *, #7898, .T. ) ;
#5532 = CARTESIAN_POINT ( 'NONE',  ( 5.257311121191341030, -73.24547149457073658, 0.09995255151718437925 ) ) ;
#5533 = CARTESIAN_POINT ( 'NONE',  ( 0.09506052544075412059, -67.99547149457075079, -4.999999999999997335 ) ) ;
#5534 = CARTESIAN_POINT ( 'NONE',  ( 3.015831842038231958, -61.80452850542926058, 3.989209796945429432 ) ) ;
#5535 = DIRECTION ( 'NONE',  ( -1.000000000000000000, -0.000000000000000000, 0.000000000000000000 ) ) ;
#5536 = CARTESIAN_POINT ( 'NONE',  ( 2.862020680886597557, -60.79547149457074084, 4.100960146803977580 ) ) ;
#5537 = ADVANCED_FACE ( 'NONE', ( #1382 ), #5886, .T. ) ;
#5538 =( NAMED_UNIT ( * ) PLANE_ANGLE_UNIT ( ) SI_UNIT ( $, .RADIAN. ) );
#5539 = CARTESIAN_POINT ( 'NONE',  ( 1.719659006605392504, -94.65452850542921226, 4.969112962950016588 ) ) ;
#5540 = ORIENTED_EDGE ( 'NONE', *, *, #3852, .T. ) ;
#5541 = UNCERTAINTY_MEASURE_WITH_UNIT (LENGTH_MEASURE( 1.000000000000000082E-05 ), #1740, 'distance_accuracy_value', 'NONE');
#5542 = DIRECTION ( 'NONE',  ( 1.000000000000000000, 0.000000000000000000, 0.000000000000000000 ) ) ;
#5543 = ORIENTED_EDGE ( 'NONE', *, *, #3004, .T. ) ;
#5544 = LINE ( 'NONE', #6136, #3421 ) ;
#5545 = CARTESIAN_POINT ( 'NONE',  ( -3.015831842038213750, -84.30452850542926058, -3.989209796945429432 ) ) ;
#5546 = CARTESIAN_POINT ( 'NONE',  ( -1.529537955723774711, -92.14547149457071384, -5.030887037049945221 ) ) ;
#5547 = CARTESIAN_POINT ( 'NONE',  ( -3.015831842038216415, -66.30452850542926058, -3.989209796945429432 ) ) ;
#5548 = AXIS2_PLACEMENT_3D ( 'NONE', #7902, #4013, #5358 ) ;
#5549 = CARTESIAN_POINT ( 'NONE',  ( -0.09506052544075593858, -81.49547149457075079, 2.999999999999997780 ) ) ;
#5550 = CARTESIAN_POINT ( 'NONE',  ( 1.840261337453218626, -61.69547149457074653, -2.371175808195584267 ) ) ;
#5551 = CARTESIAN_POINT ( 'NONE',  ( -4.725907263620322318, -66.90452850542925489, 1.635492904037698647 ) ) ;
#5552 = CARTESIAN_POINT ( 'NONE',  ( 6.628020296210642037, -83.40452850542925489, -2.253526892787612645 ) ) ;
#5553 = CARTESIAN_POINT ( 'NONE',  ( -1.840261337453197976, -96.19547149457075363, 2.371175808195584267 ) ) ;
#5554 =( NAMED_UNIT ( * ) SI_UNIT ( $, .STERADIAN. ) SOLID_ANGLE_UNIT ( ) );
#5555 = VERTEX_POINT ( 'NONE', #4493 ) ;
#5556 = LINE ( 'NONE', #2568, #5626 ) ;
#5557 = CARTESIAN_POINT ( 'NONE',  ( -0.09506052544083884448, -87.00452850542924921, -4.999999999999997335 ) ) ;
#5558 = CARTESIAN_POINT ( 'NONE',  ( 2.882544866740894829, -65.10452850542924352, 0.8366430509618999478 ) ) ;
#5559 = AXIS2_PLACEMENT_3D ( 'NONE', #1041, #2391, #4877 ) ;
#5560 = CARTESIAN_POINT ( 'NONE',  ( 0.09506052544073499699, -82.99547149457075079, -6.999999999999997335 ) ) ;
#5561 = CARTESIAN_POINT ( 'NONE',  ( -1.719659006605370744, -93.15452850542925489, -4.969112962950016588 ) ) ;
#5562 = CARTESIAN_POINT ( 'NONE',  ( 5.257311121191343695, -91.24547149457072237, 0.09995255151718437925 ) ) ;
#5563 = CARTESIAN_POINT ( 'NONE',  ( 0.09506052544084032940, -88.50452850542926342, 2.999999999999997780 ) ) ;
#5564 =( GEOMETRIC_REPRESENTATION_CONTEXT ( 3 ) GLOBAL_UNCERTAINTY_ASSIGNED_CONTEXT ( ( #8160 ) ) GLOBAL_UNIT_ASSIGNED_CONTEXT ( ( #4857, #4057, #3589 ) ) REPRESENTATION_CONTEXT ( 'NONE', 'WORKASPACE' ) );
#5565 = ORIENTED_EDGE ( 'NONE', *, *, #5753, .F. ) ;
#5566 = PRESENTATION_STYLE_ASSIGNMENT (( #4977 ) ) ;
#5567 = CARTESIAN_POINT ( 'NONE',  ( -4.312004677471060532, -60.45452850542923784, -3.009306630940844052 ) ) ;
#5568 = CARTESIAN_POINT ( 'NONE',  ( 6.628020296210686446, -73.09547149457071669, 2.253526892787472757 ) ) ;
#5569 = CARTESIAN_POINT ( 'NONE',  ( 65.00000000000000000, -7.999999999999996447, 12.49999999999999822 ) ) ;
#5570 = CARTESIAN_POINT ( 'NONE',  ( 4.784657899331177688, -79.39547149457074227, -1.454677039711874009 ) ) ;
#5571 = CARTESIAN_POINT ( 'NONE',  ( 4.194503406049401306, -72.94547149457073942, 3.171033256558012159 ) ) ;
#5572 = AXIS2_PLACEMENT_3D ( 'NONE', #5783, #7650, #11 ) ;
#5573 = CARTESIAN_POINT ( 'NONE',  ( -4.784657899331191899, -60.60452850542925773, -1.454677039711773867 ) ) ;
#5574 = LINE ( 'NONE', #4945, #7189 ) ;
#5575 = EDGE_CURVE ( 'NONE', #577, #5645, #2149, .T. ) ;
#5576 = CARTESIAN_POINT ( 'NONE',  ( -4.725907263620321430, -72.90452850542925489, 1.635492904037698647 ) ) ;
#5577 = ADVANCED_FACE ( 'NONE', ( #618 ), #3913, .T. ) ;
#5578 = CARTESIAN_POINT ( 'NONE',  ( -4.312004677470994807, -63.04547149457074084, 3.009306630940933758 ) ) ;
#5579 = ORIENTED_EDGE ( 'NONE', *, *, #3156, .F. ) ;
#5580 = DIRECTION ( 'NONE',  ( -0.000000000000000000, 1.000000000000000000, 1.387778780781445676E-16 ) ) ;
#5581 = ORIENTED_EDGE ( 'NONE', *, *, #6060, .F. ) ;
#5582 = DIRECTION ( 'NONE',  ( 0.000000000000000000, 0.000000000000000000, -1.000000000000000000 ) ) ;
#5583 = CARTESIAN_POINT ( 'NONE',  ( -1.529537955723668574, -88.35452850542925773, 5.030887037049979860 ) ) ;
#5584 = CARTESIAN_POINT ( 'NONE',  ( -4.725907263620352516, -86.59547149457075932, -1.635492904037597617 ) ) ;
#5585 = CARTESIAN_POINT ( 'NONE',  ( -5.257311121191325043, -66.75452850542924921, 0.09995255151729529053 ) ) ;
#5586 = CARTESIAN_POINT ( 'NONE',  ( 1.840261337453220625, -79.69547149457075363, -2.371175808195584267 ) ) ;
#5587 = CARTESIAN_POINT ( 'NONE',  ( 6.628020296210641149, -77.40452850542925489, -2.253526892787612645 ) ) ;
#5588 = CARTESIAN_POINT ( 'NONE',  ( 4.194503406049402194, -84.94547149457073942, 3.171033256558012159 ) ) ;
#5589 = CARTESIAN_POINT ( 'NONE',  ( 3.015831842038232402, -64.80452850542926058, 3.989209796945429432 ) ) ;
#5590 = CARTESIAN_POINT ( 'NONE',  ( 4.191402346623197772, -76.80452850542926058, 5.607243785695311900 ) ) ;
#5591 = CARTESIAN_POINT ( 'NONE',  ( -0.8796985632578817604, -58.35452850542927195, 3.030887037049973198 ) ) ;
#5592 = EDGE_LOOP ( 'NONE', ( #2471, #8176, #1943, #7923 ) ) ;
#5593 = LINE ( 'NONE', #5634, #1878 ) ;
#5594 = ORIENTED_EDGE ( 'NONE', *, *, #414, .T. ) ;
#5595 = CARTESIAN_POINT ( 'NONE',  ( 0.09506052544086235345, -94.50452850542926342, 4.999999999999997335 ) ) ;
#5596 = CARTESIAN_POINT ( 'NONE',  ( -0.8796985632578805392, -67.35452850542924352, 3.030887037049973198 ) ) ;
#5597 = EDGE_CURVE ( 'NONE', #1587, #2454, #4963, .T. ) ;
#5598 = CARTESIAN_POINT ( 'NONE',  ( 0.09506052544086235345, -94.50452850542926342, 4.999999999999997335 ) ) ;
#5599 = CARTESIAN_POINT ( 'NONE',  ( -6.013306294175060351, -78.04547149457074795, 4.245374608440741326 ) ) ;
#5600 = CARTESIAN_POINT ( 'NONE',  ( 50.00000000000000000, -20.00000000000000355, 9.499999999999998224 ) ) ;
#5601 = CARTESIAN_POINT ( 'NONE',  ( 5.257311121191343695, -88.24547149457073658, 0.09995255151718437925 ) ) ;
#5602 = CARTESIAN_POINT ( 'NONE',  ( 2.493201789345272257, -83.55452850542926058, -1.934965279058294518 ) ) ;
#5603 = CARTESIAN_POINT ( 'NONE',  ( 50.00000000000000000, -7.999999999999992895, -12.50000000000000178 ) ) ;
#5604 = EDGE_LOOP ( 'NONE', ( #6321, #2903, #2738, #6792 ) ) ;
#5605 = PLANE ( 'NONE',  #7729 ) ;
#5606 = CARTESIAN_POINT ( 'NONE',  ( -1.686450176301563353, -94.20452850542928047, 2.482926158054133303 ) ) ;
#5607 = CARTESIAN_POINT ( 'NONE',  ( 6.686770931921476979, -73.39547149457074227, -2.072711028461788896 ) ) ;
#5608 = PRODUCT_DEFINITION ( 'UNKNOWN', '', #6848, #6704 ) ;
#5609 = CARTESIAN_POINT ( 'NONE',  ( 0.000000000000000000, 0.000000000000000000, 0.000000000000000000 ) ) ;
#5610 = CARTESIAN_POINT ( 'NONE',  ( 4.315201955286068092, -96.99999999999994316, -4.064365295468459927 ) ) ;
#5611 = CARTESIAN_POINT ( 'NONE',  ( 1.719659006605284146, -64.84547149457071669, -4.969112962950050338 ) ) ;
#5612 = CARTESIAN_POINT ( 'NONE',  ( -5.257311121191324155, -65.74547149457073658, -0.09995255151718371311 ) ) ;
#5613 = CARTESIAN_POINT ( 'NONE',  ( 4.725907263620339194, -59.40452850542926200, -1.635492904037697981 ) ) ;
#5614 = CARTESIAN_POINT ( 'NONE',  ( 80.00000000000000000, 1.734723475976807094E-15, -12.50000000000000000 ) ) ;
#5615 = CARTESIAN_POINT ( 'NONE',  ( -0.09506052544084148126, -66.00452850542926342, -4.999999999999997335 ) ) ;
#5616 = CARTESIAN_POINT ( 'NONE',  ( 2.369498399071080286, -97.84547149457073090, -6.969112962950057444 ) ) ;
#5617 = EDGE_LOOP ( 'NONE', ( #5402, #6687 ) ) ;
#5618 = DIRECTION ( 'NONE',  ( 0.000000000000000000, 0.000000000000000000, 1.000000000000000000 ) ) ;
#5619 = ORIENTED_EDGE ( 'NONE', *, *, #6344, .F. ) ;
#5620 = PLANE ( 'NONE',  #6639 ) ;
#5621 = CARTESIAN_POINT ( 'NONE',  ( 1.719659006605390283, -73.65452850542924068, 4.969112962950016588 ) ) ;
#5622 = EDGE_CURVE ( 'NONE', #7927, #4976, #2545, .T. ) ;
#5623 = CARTESIAN_POINT ( 'NONE',  ( 1.719659006605286811, -88.84547149457070248, -4.969112962950050338 ) ) ;
#5624 = CARTESIAN_POINT ( 'NONE',  ( -4.312004677471058756, -60.45452850542924494, -3.009306630940843608 ) ) ;
#5625 = CARTESIAN_POINT ( 'NONE',  ( -0.09506052544075706268, -72.49547149457075079, 2.999999999999997780 ) ) ;
#5626 = VECTOR ( 'NONE', #6525, 1000.000000000000000 ) ;
#5627 = CARTESIAN_POINT ( 'NONE',  ( -5.895805022753386027, -82.05452850542926058, 4.407101234057909878 ) ) ;
#5628 = CARTESIAN_POINT ( 'NONE',  ( -4.194503406049382654, -89.44547149457073942, -3.171033256558012159 ) ) ;
#5629 = CARTESIAN_POINT ( 'NONE',  ( -4.784657899331191011, -69.60452850542925773, -1.454677039711773867 ) ) ;
#5630 = CARTESIAN_POINT ( 'NONE',  ( -6.686770931921506289, -75.60452850542924352, -2.072711028461647675 ) ) ;
#5631 = CARTESIAN_POINT ( 'NONE',  ( 2.882544866740878842, -88.39547149457074227, -0.8366430509619593447 ) ) ;
#5632 = AXIS2_PLACEMENT_3D ( 'NONE', #1900, #1940, #5172 ) ;
#5633 = ORIENTED_EDGE ( 'NONE', *, *, #5827, .F. ) ;
#5634 = CARTESIAN_POINT ( 'NONE',  ( 80.00000000000000000, 0.000000000000000000, 20.00000000000000000 ) ) ;
#5635 = CARTESIAN_POINT ( 'NONE',  ( 0.09506052544075295485, -58.99547149457073658, -4.999999999999997335 ) ) ;
#5636 = VERTEX_POINT ( 'NONE', #7667 ) ;
#5637 = CARTESIAN_POINT ( 'NONE',  ( 1.719659006605392504, -91.65452850542925489, 4.969112962950015699 ) ) ;
#5638 = CARTESIAN_POINT ( 'NONE',  ( 2.610703060766983441, -70.95452850542925205, 1.773238653441072232 ) ) ;
#5639 = ORIENTED_EDGE ( 'NONE', *, *, #7587, .T. ) ;
#5640 = EDGE_CURVE ( 'NONE', #1530, #1162, #578, .T. ) ;
#5641 = CARTESIAN_POINT ( 'NONE',  ( 6.686770931921522276, -59.10452850542926484, 2.072711028461649008 ) ) ;
#5642 = CARTESIAN_POINT ( 'NONE',  ( 6.686770931921476979, -73.39547149457074227, -2.072711028461788896 ) ) ;
#5643 = CARTESIAN_POINT ( 'NONE',  ( 2.862020680886601109, -90.79547149457074795, 4.100960146803977580 ) ) ;
#5644 = CARTESIAN_POINT ( 'NONE',  ( 2.882544866740897049, -77.10452850542924352, 0.8366430509618999478 ) ) ;
#5645 = VERTEX_POINT ( 'NONE', #2699 ) ;
#5646 =( NAMED_UNIT ( * ) SI_UNIT ( $, .STERADIAN. ) SOLID_ANGLE_UNIT ( ) );
#5647 = CARTESIAN_POINT ( 'NONE',  ( -0.09506052544084186984, -63.00452850542925631, -4.999999999999997335 ) ) ;
#5648 = CARTESIAN_POINT ( 'NONE',  ( -0.09506052544071454113, -72.49547149457075079, 6.999999999999997335 ) ) ;
#5649 = CARTESIAN_POINT ( 'NONE',  ( 5.679463638039127460, -97.00000000000000000, -1.065672799591116826 ) ) ;
#5650 = CARTESIAN_POINT ( 'NONE',  ( -4.312004677470994807, -63.04547149457073374, 3.009306630940933314 ) ) ;
#5651 = CARTESIAN_POINT ( 'NONE',  ( 4.725907263620371168, -64.09547149457073090, 1.635492904037598283 ) ) ;
#5652 = CARTESIAN_POINT ( 'NONE',  ( -3.154386672714787565, -90.75452850542924921, 0.09995255151727280851 ) ) ;
#5653 = LINE ( 'NONE', #2585, #1112 ) ;
#5654 = CARTESIAN_POINT ( 'NONE',  ( -2.862020680886495860, -64.20452850542926626, 4.100960146804039752 ) ) ;
#5655 = CARTESIAN_POINT ( 'NONE',  ( -6.013306294175056799, -96.04547149457074795, 4.245374608440741326 ) ) ;
#5656 = SURFACE_STYLE_USAGE ( .BOTH. , #399 ) ;
#5657 = EDGE_LOOP ( 'NONE', ( #3563, #1731, #705, #2310 ) ) ;
#5658 = FACE_BOUND ( 'NONE', #6568, .T. ) ;
#5659 = ORIENTED_EDGE ( 'NONE', *, *, #7003, .T. ) ;
#5660 = CARTESIAN_POINT ( 'NONE',  ( 50.00000000000000000, -19.99999999999999645, -12.50000000000000355 ) ) ;
#5661 = CARTESIAN_POINT ( 'NONE',  ( -4.725907263620321430, -75.90452850542925489, 1.635492904037698647 ) ) ;
#5662 = CARTESIAN_POINT ( 'NONE',  ( 5.257311121191342806, -94.24547149457070816, 0.09995255151718437925 ) ) ;
#5663 = CARTESIAN_POINT ( 'NONE',  ( 1.719659006605388951, -61.65452850542924779, 4.969112962950015699 ) ) ;
#5664 = CARTESIAN_POINT ( 'NONE',  ( 1.840261337453219515, -70.69547149457073942, -2.371175808195584267 ) ) ;
#5665 = CARTESIAN_POINT ( 'NONE',  ( -2.179377348189461383, -79.35452850542927195, 7.030887037049988741 ) ) ;
#5666 = CARTESIAN_POINT ( 'NONE',  ( -5.257311121191322378, -89.74547149457070816, -0.09995255151718371311 ) ) ;
#5667 = CARTESIAN_POINT ( 'NONE',  ( 1.529537955723689224, -68.85452850542921510, -5.030887037049978971 ) ) ;
#5668 = CARTESIAN_POINT ( 'NONE',  ( -4.037591185471422150, -82.20452850542925205, 5.718994135553947977 ) ) ;
#5669 = CARTESIAN_POINT ( 'NONE',  ( -0.09506052544075556388, -84.49547149457075079, 2.999999999999997780 ) ) ;
#5670 = ORIENTED_EDGE ( 'NONE', *, *, #903, .T. ) ;
#5671 = CARTESIAN_POINT ( 'NONE',  ( 47.49999999999999289, -20.00000000000000355, 12.49999999999999112 ) ) ;
#5672 = CARTESIAN_POINT ( 'NONE',  ( 80.00000000000000000, -19.99999999999999645, -12.50000000000000355 ) ) ;
#5673 = ORIENTED_EDGE ( 'NONE', *, *, #4088, .T. ) ;
#5674 = CARTESIAN_POINT ( 'NONE',  ( -4.784657899331188347, -93.60452850542925773, -1.454677039711773867 ) ) ;
#5675 = CARTESIAN_POINT ( 'NONE',  ( -1.686450176301567572, -61.20452850542925916, 2.482926158054133303 ) ) ;
#5676 = EDGE_CURVE ( 'NONE', #4159, #2855, #3199, .T. ) ;
#5677 = CARTESIAN_POINT ( 'NONE',  ( 4.784657899331212327, -95.10452850542925773, 1.454677039711774533 ) ) ;
#5678 = CARTESIAN_POINT ( 'NONE',  ( -6.628020296210667794, -71.59547149457071669, -2.253526892787471869 ) ) ;
#5679 = CARTESIAN_POINT ( 'NONE',  ( 4.194503406049403083, -90.94547149457072521, 3.171033256558012159 ) ) ;
#5680 = CARTESIAN_POINT ( 'NONE',  ( 3.154386672714809325, -80.25452850542926342, -0.09995255151727241993 ) ) ;
#5681 = LINE ( 'NONE', #3799, #4030 ) ;
#5682 = VERTEX_POINT ( 'NONE', #4449 ) ;
#5683 = CARTESIAN_POINT ( 'NONE',  ( -47.50000000000000711, -51.00000000000000711, 12.50000000000001954 ) ) ;
#5684 = CARTESIAN_POINT ( 'NONE',  ( -1.686450176301564019, -91.20452850542925205, 2.482926158054133303 ) ) ;
#5685 = CARTESIAN_POINT ( 'NONE',  ( -4.191402346623060104, -63.19547149457074653, 5.607243785695398941 ) ) ;
#5686 = PLANE ( 'NONE',  #2684 ) ;
#5687 = CARTESIAN_POINT ( 'NONE',  ( 4.194503406049401306, -69.94547149457072521, 3.171033256558012159 ) ) ;
#5688 = CARTESIAN_POINT ( 'NONE',  ( -2.179377348189608821, -95.14547149457074227, -7.030887037049939003 ) ) ;
#5689 = CARTESIAN_POINT ( 'NONE',  ( -2.823794231030019031, -93.90452850542926910, 1.017458915287783316 ) ) ;
#5690 = DIRECTION ( 'NONE',  ( 0.5000000000000011102, -0.8660254037844380415, 0.000000000000000000 ) ) ;
#5691 = AXIS2_PLACEMENT_3D ( 'NONE', #7204, #3329, #2151 ) ;
#5692 = VECTOR ( 'NONE', #1970, 1000.000000000000000 ) ;
#5693 = CARTESIAN_POINT ( 'NONE',  ( 4.194503406049335581, -68.55452850542926058, -3.171033256558100089 ) ) ;
#5694 = CARTESIAN_POINT ( 'NONE',  ( -4.037591185471542055, -95.29547149457076216, -5.718994135553860936 ) ) ;
#5695 = CIRCLE ( 'NONE', #2762, 1.499999999999994449 ) ;
#5696 = EDGE_LOOP ( 'NONE', ( #5464, #3868 ) ) ;
#5697 = EDGE_CURVE ( 'NONE', #981, #5461, #3869, .T. ) ;
#5698 = DIRECTION ( 'NONE',  ( 1.000000000000000000, -0.000000000000000000, -0.000000000000000000 ) ) ;
#5699 = AXIS2_PLACEMENT_3D ( 'NONE', #6884, #2311, #1799 ) ;
#5700 = ORIENTED_EDGE ( 'NONE', *, *, #3359, .F. ) ;
#5701 = LINE ( 'NONE', #8282, #2755 ) ;
#5702 = CARTESIAN_POINT ( 'NONE',  ( 1.529537955723689890, -74.85452850542925773, -5.030887037049978971 ) ) ;
#5703 = CARTESIAN_POINT ( 'NONE',  ( 4.784657899331178577, -85.39547149457074227, -1.454677039711874009 ) ) ;
#5704 = CARTESIAN_POINT ( 'NONE',  ( 50.00000000000000000, -20.00000000000000355, 12.49999999999999645 ) ) ;
#5705 = CARTESIAN_POINT ( 'NONE',  ( 2.493201789345310004, -75.94547149457073942, 1.934965279058241006 ) ) ;
#5706 = CARTESIAN_POINT ( 'NONE',  ( -6.628020296210620721, -81.90452850542925489, 2.253526892787613978 ) ) ;
#5707 = PRODUCT_RELATED_PRODUCT_CATEGORY ( 'part', '', ( #1788 ) ) ;
#5708 = CARTESIAN_POINT ( 'NONE',  ( 1.529537955723796916, -90.64547149457075648, 5.030887037049945221 ) ) ;
#5709 = FACE_OUTER_BOUND ( 'NONE', #7229, .T. ) ;
#5710 = CARTESIAN_POINT ( 'NONE',  ( -5.895805022753386027, -76.05452850542926058, 4.407101234057909878 ) ) ;
#5711 = CARTESIAN_POINT ( 'NONE',  ( 2.610703060766946582, -88.54547149457074795, -1.773238653441125523 ) ) ;
#5712 = ADVANCED_FACE ( 'NONE', ( #659, #3242 ), #5798, .T. ) ;
#5713 = ORIENTED_EDGE ( 'NONE', *, *, #6870, .F. ) ;
#5714 =( REPRESENTATION_RELATIONSHIP ('NONE','NONE', #4188, #153 ) REPRESENTATION_RELATIONSHIP_WITH_TRANSFORMATION ( #5961 )SHAPE_REPRESENTATION_RELATIONSHIP( ) );
#5715 = DIRECTION ( 'NONE',  ( -0.000000000000000000, -0.000000000000000000, -1.000000000000000000 ) ) ;
#5716 = FACE_OUTER_BOUND ( 'NONE', #5604, .T. ) ;
#5717 = ORIENTED_EDGE ( 'NONE', *, *, #6924, .T. ) ;
#5718 = CARTESIAN_POINT ( 'NONE',  ( -3.015831842038213750, -87.30452850542926058, -3.989209796945429432 ) ) ;
#5719 = CARTESIAN_POINT ( 'NONE',  ( 1.686450176301638626, -96.79547149457073374, 2.482926158054096000 ) ) ;
#5720 = CARTESIAN_POINT ( 'NONE',  ( 4.037591185471440802, -59.70452850542925916, -5.718994135553947977 ) ) ;
#5721 = CARTESIAN_POINT ( 'NONE',  ( -4.037591185471545607, -68.29547149457073374, -5.718994135553860936 ) ) ;
#5722 = CARTESIAN_POINT ( 'NONE',  ( 2.862020680886600665, -87.79547149457074795, 4.100960146803977580 ) ) ;
#5723 = CARTESIAN_POINT ( 'NONE',  ( -1.840261337453251489, -78.30452850542926058, -2.371175808195547852 ) ) ;
#5724 = EDGE_CURVE ( 'NONE', #731, #4167, #2683, .T. ) ;
#5725 = CYLINDRICAL_SURFACE ( 'NONE', #6587, 1.500000000000001998 ) ;
#5726 = CARTESIAN_POINT ( 'NONE',  ( -0.09506052544081780575, -87.00452850542926342, -2.999999999999997780 ) ) ;
#5727 = CARTESIAN_POINT ( 'NONE',  ( 0.09506052544073198551, -58.99547149457073658, -6.999999999999997335 ) ) ;
#5728 = DIRECTION ( 'NONE',  ( 1.000000000000000000, 0.000000000000000000, 0.000000000000000000 ) ) ;
#5729 = CARTESIAN_POINT ( 'NONE',  ( -2.862020680886581570, -68.29547149457074795, -4.100960146803977580 ) ) ;
#5730 = CARTESIAN_POINT ( 'NONE',  ( 0.09506052544073653743, -94.99547149457075079, -6.999999999999997335 ) ) ;
#5731 = CARTESIAN_POINT ( 'NONE',  ( 2.882544866740898382, -92.10452850542925773, 0.8366430509618999478 ) ) ;
#5732 = DIRECTION ( 'NONE',  ( -0.000000000000000000, 0.7071067811865484609, -0.7071067811865465735 ) ) ;
#5733 = CARTESIAN_POINT ( 'NONE',  ( 4.312004677471074743, -67.95452850542922363, 3.009306630940844496 ) ) ;
#5734 = CARTESIAN_POINT ( 'NONE',  ( -4.037591185471542943, -92.29547149457074795, -5.718994135553860936 ) ) ;
#5735 = PRESENTATION_STYLE_ASSIGNMENT (( #730 ) ) ;
#5736 = ORIENTED_EDGE ( 'NONE', *, *, #8239, .F. ) ;
#5737 = LINE ( 'NONE', #1324, #5031 ) ;
#5738 = PRODUCT_DEFINITION_SHAPE ( 'NONE', 'NONE',  #8345 ) ;
#5739 = PRODUCT_CONTEXT ( 'NONE', #992, 'mechanical' ) ;
#5740 = VERTEX_POINT ( 'NONE', #7794 ) ;
#5741 = AXIS2_PLACEMENT_3D ( 'NONE', #3944, #4567, #4526 ) ;
#5742 = FACE_OUTER_BOUND ( 'NONE', #2170, .T. ) ;
#5743 = CARTESIAN_POINT ( 'NONE',  ( -4.312004677471056979, -81.45452850542923784, -3.009306630940844052 ) ) ;
#5744 = CARTESIAN_POINT ( 'NONE',  ( -5.257311121191324155, -77.74547149457070816, -0.09995255151718371311 ) ) ;
#5745 = CARTESIAN_POINT ( 'NONE',  ( 3.640901902936454437, -96.99999999999988631, -1.978986728491922920 ) ) ;
#5746 = CARTESIAN_POINT ( 'NONE',  ( 0.8796985632579609193, -69.64547149457072805, 3.030887037049952326 ) ) ;
#5747 = CARTESIAN_POINT ( 'NONE',  ( -6.628020296210620721, -78.90452850542925489, 2.253526892787613978 ) ) ;
#5748 = CARTESIAN_POINT ( 'NONE',  ( 1.719659006605285478, -73.84547149457074511, -4.969112962950050338 ) ) ;
#5749 = CARTESIAN_POINT ( 'NONE',  ( -47.50000000000000711, -198.2344135219424857, -12.50000000000005151 ) ) ;
#5750 = CARTESIAN_POINT ( 'NONE',  ( 4.312004677471079184, -94.95452850542926626, 3.009306630940844496 ) ) ;
#5751 = CARTESIAN_POINT ( 'NONE',  ( 6.686770931921524941, -80.10452850542927195, 2.072711028461649008 ) ) ;
#5752 = CARTESIAN_POINT ( 'NONE',  ( 1.069819614139496000, -88.84547149457073090, -2.969112962950042789 ) ) ;
#5753 = EDGE_CURVE ( 'NONE', #5461, #7447, #1342, .T. ) ;
#5754 = ORIENTED_EDGE ( 'NONE', *, *, #7828, .F. ) ;
#5755 = FACE_OUTER_BOUND ( 'NONE', #7669, .T. ) ;
#5756 = CARTESIAN_POINT ( 'NONE',  ( 54.99999999999999289, -9.999999999999994671, 0.000000000000000000 ) ) ;
#5757 = ORIENTED_EDGE ( 'NONE', *, *, #6898, .T. ) ;
#5758 = CARTESIAN_POINT ( 'NONE',  ( -3.015831842038213750, -84.30452850542926058, -3.989209796945429432 ) ) ;
#5759 = CARTESIAN_POINT ( 'NONE',  ( -1.840261337453197976, -96.19547149457075363, 2.371175808195584267 ) ) ;
#5760 = CARTESIAN_POINT ( 'NONE',  ( 2.369498399071222838, -58.65452850542925489, 6.969112962950009482 ) ) ;
#5761 = CARTESIAN_POINT ( 'NONE',  ( 2.369498399071076733, -70.84547149457073090, -6.969112962950057444 ) ) ;
#5762 = EDGE_CURVE ( 'NONE', #6651, #7734, #747, .T. ) ;
#5763 = VECTOR ( 'NONE', #3745, 1000.000000000000000 ) ;
#5764 = CARTESIAN_POINT ( 'NONE',  ( -4.725907263620352516, -83.59547149457074511, -1.635492904037597617 ) ) ;
#5765 = CARTESIAN_POINT ( 'NONE',  ( 1.840261337453270585, -73.80452850542926058, 2.371175808195547852 ) ) ;
#5766 = APPLICATION_CONTEXT ( 'automotive_design' ) ;
#5767 = CARTESIAN_POINT ( 'NONE',  ( 43.45299461620744097, 100.0000000000000000, 7.500000000000000000 ) ) ;
#5768 = AXIS2_PLACEMENT_3D ( 'NONE', #753, #3334, #5892 ) ;
#5769 = FACE_OUTER_BOUND ( 'NONE', #6695, .T. ) ;
#5770 = CARTESIAN_POINT ( 'NONE',  ( -2.493201789345250940, -85.05452850542926058, 1.934965279058294518 ) ) ;
#5771 = CARTESIAN_POINT ( 'NONE',  ( -5.895805022753480173, -59.44547149457074653, -4.407101234057782868 ) ) ;
#5772 = DIRECTION ( 'NONE',  ( 0.000000000000000000, -1.000000000000000000, -2.168404344971010347E-16 ) ) ;
#5773 = CARTESIAN_POINT ( 'NONE',  ( 4.784657899331175912, -64.39547149457074227, -1.454677039711874009 ) ) ;
#5774 = CARTESIAN_POINT ( 'NONE',  ( -1.529537955723778486, -62.14547149457074227, -5.030887037049945221 ) ) ;
#5775 = DIRECTION ( 'NONE',  ( 0.000000000000000000, -1.734723475976807094E-16, 1.000000000000000000 ) ) ;
#5776 = CARTESIAN_POINT ( 'NONE',  ( -47.50000000000002132, -97.00000000000000000, 12.49999999999996803 ) ) ;
#5777 = VECTOR ( 'NONE', #5331, 1000.000000000000000 ) ;
#5778 = CARTESIAN_POINT ( 'NONE',  ( 4.312004677471073855, -61.95452850542923784, 3.009306630940844496 ) ) ;
#5779 =( GEOMETRIC_REPRESENTATION_CONTEXT ( 3 ) GLOBAL_UNCERTAINTY_ASSIGNED_CONTEXT ( ( #6036 ) ) GLOBAL_UNIT_ASSIGNED_CONTEXT ( ( #772, #1493, #6712 ) ) REPRESENTATION_CONTEXT ( 'NONE', 'WORKASPACE' ) );
#5780 = CARTESIAN_POINT ( 'NONE',  ( 7.360235569667880284, -91.24547149457073658, 0.09995255151716216091 ) ) ;
#5781 = VERTEX_POINT ( 'NONE', #2026 ) ;
#5782 = CARTESIAN_POINT ( 'NONE',  ( -4.784657899331190123, -78.60452850542925773, -1.454677039711773867 ) ) ;
#5783 = CARTESIAN_POINT ( 'NONE',  ( 45.00000000000000000, -14.99999999999999467, 4.499999999999999112 ) ) ;
#5784 = PRODUCT_CONTEXT ( 'NONE', #883, 'mechanical' ) ;
#5785 = ADVANCED_FACE ( 'NONE', ( #4575, #7159 ), #6400, .T. ) ;
#5786 = DIRECTION ( 'NONE',  ( 1.000000000000000000, 0.000000000000000000, -0.000000000000000000 ) ) ;
#5787 = CARTESIAN_POINT ( 'NONE',  ( 4.312004677471012570, -76.54547149457071953, -3.009306630940933314 ) ) ;
#5788 = PLANE ( 'NONE',  #8078 ) ;
#5789 = CARTESIAN_POINT ( 'NONE',  ( 0.09506052544077515931, -67.99547149457075079, -2.999999999999997780 ) ) ;
#5790 = CARTESIAN_POINT ( 'NONE',  ( 7.360235569667877620, -65.25452850542926342, -0.09995255151731691212 ) ) ;
#5791 = CARTESIAN_POINT ( 'NONE',  ( 6.000000000000011546, -100.0010000000000048, -2.499999999999999112 ) ) ;
#5792 = CARTESIAN_POINT ( 'NONE',  ( -0.09506052544073466393, -81.49547149457075079, 4.999999999999997335 ) ) ;
#5793 = DIRECTION ( 'NONE',  ( 1.000000000000000000, 0.000000000000000000, -0.000000000000000000 ) ) ;
#5794 = CARTESIAN_POINT ( 'NONE',  ( 0.09506052544086197875, -91.50452850542924921, 4.999999999999997335 ) ) ;
#5795 = CARTESIAN_POINT ( 'NONE',  ( -2.179377348189461827, -70.35452850542922931, 7.030887037049988741 ) ) ;
#5796 = CARTESIAN_POINT ( 'NONE',  ( 1.686450176301637960, -90.79547149457074795, 2.482926158054096000 ) ) ;
#5797 = ORIENTED_EDGE ( 'NONE', *, *, #8014, .T. ) ;
#5798 = PLANE ( 'NONE',  #4287 ) ;
#5799 = CARTESIAN_POINT ( 'NONE',  ( -47.50000000000000711, 47.23441352194253540, -12.50000000000001954 ) ) ;
#5800 = CARTESIAN_POINT ( 'NONE',  ( 4.725907263620341858, -92.40452850542925489, -1.635492904037697981 ) ) ;
#5801 = ORIENTED_EDGE ( 'NONE', *, *, #1229, .F. ) ;
#5802 = CARTESIAN_POINT ( 'NONE',  ( -4.784657899331190123, -81.60452850542925773, -1.454677039711773867 ) ) ;
#5803 = CARTESIAN_POINT ( 'NONE',  ( 2.823794231030038571, -62.40452850542925489, -1.017458915287783316 ) ) ;
#5804 = DIRECTION ( 'NONE',  ( 0.000000000000000000, 0.000000000000000000, 1.000000000000000000 ) ) ;
#5805 = CARTESIAN_POINT ( 'NONE',  ( 2.862020680886515400, -86.70452850542925205, -4.100960146804039752 ) ) ;
#5806 = CARTESIAN_POINT ( 'NONE',  ( -2.179377348189612373, -68.14547149457074227, -7.030887037049939003 ) ) ;
#5807 = CARTESIAN_POINT ( 'NONE',  ( -0.09506052544073466393, -81.49547149457075079, 4.999999999999997335 ) ) ;
#5808 = CARTESIAN_POINT ( 'NONE',  ( 2.493201789345271369, -71.55452850542926058, -1.934965279058294518 ) ) ;
#5809 = CARTESIAN_POINT ( 'NONE',  ( 54.99999999999999289, 50.00000000000000000, 7.500000000000000000 ) ) ;
#5810 = CARTESIAN_POINT ( 'NONE',  ( 43.45299461620744097, 100.0000000000000000, 7.500000000000000000 ) ) ;
#5811 = CARTESIAN_POINT ( 'NONE',  ( 0.8796985632579000791, -86.85452850542924352, -3.030887037049972310 ) ) ;
#5812 = CARTESIAN_POINT ( 'NONE',  ( -6.686770931921461880, -59.89547149457074937, 2.072711028461789784 ) ) ;
#5813 = VECTOR ( 'NONE', #7178, 1000.000000000000000 ) ;
#5814 = CARTESIAN_POINT ( 'NONE',  ( 50.00000000000000000, -9.999999999999994671, 10.50000000000000533 ) ) ;
#5815 = CARTESIAN_POINT ( 'NONE',  ( 5.257311121191341918, -80.25452850542922079, -0.09995255151729465215 ) ) ;
#5816 = CARTESIAN_POINT ( 'NONE',  ( -6.628020296210665130, -95.59547149457074511, -2.253526892787471869 ) ) ;
#5817 = DIRECTION ( 'NONE',  ( 1.000000000000000000, 0.000000000000000000, 0.000000000000000000 ) ) ;
#5818 = FACE_BOUND ( 'NONE', #1222, .T. ) ;
#5819 = CARTESIAN_POINT ( 'NONE',  ( -4.784657899331192787, -57.60452850542925773, -1.454677039711773867 ) ) ;
#5820 = CARTESIAN_POINT ( 'NONE',  ( -2.369498399071055861, -87.34547149457073090, 6.969112962950058332 ) ) ;
#5821 = SURFACE_STYLE_USAGE ( .BOTH. , #3265 ) ;
#5822 = EDGE_LOOP ( 'NONE', ( #6359, #3525, #6764, #143 ) ) ;
#5823 = CARTESIAN_POINT ( 'NONE',  ( 4.194503406049335581, -71.55452850542926058, -3.171033256558100089 ) ) ;
#5824 = STYLED_ITEM ( 'NONE', ( #7385 ), #4428 ) ;
#5825 = CARTESIAN_POINT ( 'NONE',  ( -54.99999999999999289, -97.00000000000000000, 20.00000000000000000 ) ) ;
#5826 = CIRCLE ( 'NONE', #3146, 1.500000000000000666 ) ;
#5827 = EDGE_CURVE ( 'NONE', #5503, #1673, #7839, .T. ) ;
#5828 = AXIS2_PLACEMENT_3D ( 'NONE', #2891, #1627, #948 ) ;
#5829 = CIRCLE ( 'NONE', #700, 4.999999999999999112 ) ;
#5830 = CARTESIAN_POINT ( 'NONE',  ( -54.99999999999999289, -100.0000000000000000, 20.00000000000000000 ) ) ;
#5831 = CIRCLE ( 'NONE', #3295, 1.499999999999994449 ) ;
#5832 = AXIS2_PLACEMENT_3D ( 'NONE', #1783, #7636, #3127 ) ;
#5833 = CARTESIAN_POINT ( 'NONE',  ( -3.015831842038128041, -84.19547149457073942, 3.989209796945492048 ) ) ;
#5834 = DIRECTION ( 'NONE',  ( -0.000000000000000000, 0.7071067811865507924, 0.7071067811865441310 ) ) ;
#5835 = CARTESIAN_POINT ( 'NONE',  ( 1.686450176301633963, -60.79547149457074084, 2.482926158054096000 ) ) ;
#5836 = CARTESIAN_POINT ( 'NONE',  ( -2.369498399071207739, -72.15452850542922647, -6.969112962950009482 ) ) ;
#5837 = CARTESIAN_POINT ( 'NONE',  ( -1.500000000000001332, -27.00000000000000000, 4.500000000000000888 ) ) ;
#5838 = CARTESIAN_POINT ( 'NONE',  ( -5.257311121191324155, -80.74547149457075079, -0.09995255151718371311 ) ) ;
#5839 = CARTESIAN_POINT ( 'NONE',  ( 4.784657899331207886, -62.10452850542925063, 1.454677039711774533 ) ) ;
#5840 = CARTESIAN_POINT ( 'NONE',  ( 4.725907263620341858, -89.40452850542926910, -1.635492904037697981 ) ) ;
#5841 = CARTESIAN_POINT ( 'NONE',  ( -6.686770931921506289, -72.60452850542924352, -2.072711028461647675 ) ) ;
#5842 = AXIS2_PLACEMENT_3D ( 'NONE', #4826, #5618, #8082 ) ;
#5843 = CARTESIAN_POINT ( 'NONE',  ( 1.840261337453220625, -79.69547149457075363, -2.371175808195584267 ) ) ;
#5844 = VERTEX_POINT ( 'NONE', #6360 ) ;
#5845 = CARTESIAN_POINT ( 'NONE',  ( 6.000000000000006217, -47.00000000000000000, -2.499999999999999112 ) ) ;
#5846 = CARTESIAN_POINT ( 'NONE',  ( 4.312004677471079184, -94.95452850542926626, 3.009306630940844496 ) ) ;
#5847 = CARTESIAN_POINT ( 'NONE',  ( -2.862020680886492752, -88.20452850542925205, 4.100960146804039752 ) ) ;
#5848 = VERTEX_POINT ( 'NONE', #2523 ) ;
#5849 = CARTESIAN_POINT ( 'NONE',  ( 2.862020680886514956, -80.70452850542925205, -4.100960146804039752 ) ) ;
#5850 = CARTESIAN_POINT ( 'NONE',  ( -2.823794231030038571, -95.59547149457074511, -1.017458915287723364 ) ) ;
#5851 = DIRECTION ( 'NONE',  ( 0.000000000000000000, 0.000000000000000000, -1.000000000000000000 ) ) ;
#5852 = CARTESIAN_POINT ( 'NONE',  ( 3.015831842038234623, -82.80452850542926058, 3.989209796945429432 ) ) ;
#5853 = CARTESIAN_POINT ( 'NONE',  ( -4.191402346623060104, -60.19547149457074653, 5.607243785695398941 ) ) ;
#5854 = CARTESIAN_POINT ( 'NONE',  ( 1.840261337453269919, -70.80452850542926058, 2.371175808195547852 ) ) ;
#5855 = FACE_BOUND ( 'NONE', #5074, .T. ) ;
#5856 = LINE ( 'NONE', #6536, #2553 ) ;
#5857 = CARTESIAN_POINT ( 'NONE',  ( -1.069819614139537078, -87.15452850542926910, -2.969112962950023249 ) ) ;
#5858 = CARTESIAN_POINT ( 'NONE',  ( 5.895805022753409119, -95.55452850542926058, -4.407101234057908989 ) ) ;
#5859 = CARTESIAN_POINT ( 'NONE',  ( 6.000000000000004441, -27.99999999999999645, 2.500000000000000888 ) ) ;
#5860 = CARTESIAN_POINT ( 'NONE',  ( -1.719659006605372076, -75.15452850542925489, -4.969112962950016588 ) ) ;
#5861 = CARTESIAN_POINT ( 'NONE',  ( 6.013306294175080779, -91.54547149457074795, -4.245374608440741326 ) ) ;
#5862 = CARTESIAN_POINT ( 'NONE',  ( -80.00000000000000000, -20.00000000000000355, 12.49999999999999645 ) ) ;
#5863 = DIRECTION ( 'NONE',  ( 0.000000000000000000, 0.000000000000000000, 1.000000000000000000 ) ) ;
#5864 = CARTESIAN_POINT ( 'NONE',  ( -4.194503406049320482, -61.05452850542923926, 3.171033256558100533 ) ) ;
#5865 = PRODUCT_DEFINITION ( 'UNKNOWN', '', #5369, #3509 ) ;
#5866 = CARTESIAN_POINT ( 'NONE',  ( 6.628020296210689111, -91.09547149457074511, 2.253526892787472757 ) ) ;
#5867 = ORIENTED_EDGE ( 'NONE', *, *, #2532, .F. ) ;
#5868 = CARTESIAN_POINT ( 'NONE',  ( -4.725907263620321430, -75.90452850542925489, 1.635492904037698647 ) ) ;
#5869 = FACE_OUTER_BOUND ( 'NONE', #3553, .T. ) ;
#5870 = CONTEXT_DEPENDENT_SHAPE_REPRESENTATION ( #5293, #7031 ) ;
#5871 = DIRECTION ( 'NONE',  ( 0.000000000000000000, 0.000000000000000000, -1.000000000000000000 ) ) ;
#5872 = ADVANCED_FACE ( 'NONE', ( #5755 ), #7944, .F. ) ;
#5873 = CARTESIAN_POINT ( 'NONE',  ( -4.725907263620353405, -80.59547149457074511, -1.635492904037597617 ) ) ;
#5874 = CARTESIAN_POINT ( 'NONE',  ( 80.00000000000000000, -9.999999999999991118, -10.50000000000000888 ) ) ;
#5875 = CARTESIAN_POINT ( 'NONE',  ( -0.09506052544075858923, -60.49547149457073658, 2.999999999999997780 ) ) ;
#5876 = CARTESIAN_POINT ( 'NONE',  ( 5.895805022753404678, -71.55452850542926058, -4.407101234057908989 ) ) ;
#5877 = CARTESIAN_POINT ( 'NONE',  ( 75.00000000000000000, -9.999999999999994671, 0.000000000000000000 ) ) ;
#5878 = CARTESIAN_POINT ( 'NONE',  ( -2.862020680886580681, -77.29547149457074795, -4.100960146803977580 ) ) ;
#5879 = APPLICATION_CONTEXT ( 'automotive_design' ) ;
#5880 = DIRECTION ( 'NONE',  ( 1.000000000000000000, 0.000000000000000000, -0.000000000000000000 ) ) ;
#5881 = CARTESIAN_POINT ( 'NONE',  ( -2.862020680886493196, -85.20452850542925205, 4.100960146804039752 ) ) ;
#5882 = CARTESIAN_POINT ( 'NONE',  ( 7.360235569667877620, -71.25452850542926342, -0.09995255151731691212 ) ) ;
#5883 = CARTESIAN_POINT ( 'NONE',  ( -1.686450176301617310, -74.29547149457074795, -2.482926158054096000 ) ) ;
#5884 = COLOUR_RGB ( '', 0.09019608, 0.27058824, 0.51372549) ;
#5885 = ORIENTED_EDGE ( 'NONE', *, *, #6840, .T. ) ;
#5886 = CYLINDRICAL_SURFACE ( 'NONE', #7525, 6.000000000000000000 ) ;
#5887 = CARTESIAN_POINT ( 'NONE',  ( -47.50000000000000711, -54.00000000000000711, -12.50000000000001954 ) ) ;
#5888 = CARTESIAN_POINT ( 'NONE',  ( 4.194503406049339134, -92.55452850542924637, -3.171033256558100089 ) ) ;
#5889 = VERTEX_POINT ( 'NONE', #1508 ) ;
#5890 = CARTESIAN_POINT ( 'NONE',  ( -4.312004677471056979, -81.45452850542923784, -3.009306630940843608 ) ) ;
#5891 = CARTESIAN_POINT ( 'NONE',  ( 3.154386672714810658, -88.24547149457073658, 0.09995255151720662534 ) ) ;
#5892 = DIRECTION ( 'NONE',  ( -0.6103455414686667080, -0.7921352914807673340, -7.499539956105955623E-49 ) ) ;
#5893 = CARTESIAN_POINT ( 'NONE',  ( -3.015831842038213750, -84.30452850542926058, -3.989209796945429432 ) ) ;
#5894 = CARTESIAN_POINT ( 'NONE',  ( 5.895805022753409119, -95.55452850542926058, -4.407101234057908989 ) ) ;
#5895 = CARTESIAN_POINT ( 'NONE',  ( 2.610703060766982553, -64.95452850542926626, 1.773238653441072232 ) ) ;
#5896 = LINE ( 'NONE', #7717, #1202 ) ;
#5897 = EDGE_CURVE ( 'NONE', #2766, #204, #8004, .T. ) ;
#5898 = CARTESIAN_POINT ( 'NONE',  ( 65.00000000000000000, -7.999999999999992895, -12.50000000000000178 ) ) ;
#5899 = CARTESIAN_POINT ( 'NONE',  ( 0.09506052544083844202, -73.50452850542924921, 2.999999999999997780 ) ) ;
#5900 = CARTESIAN_POINT ( 'NONE',  ( -4.191402346623178232, -84.30452850542926058, -5.607243785695311900 ) ) ;
#5901 = AXIS2_PLACEMENT_3D ( 'NONE', #4533, #7114, #7029 ) ;
#5902 = CYLINDRICAL_SURFACE ( 'NONE', #6983, 1.500000000000001776 ) ;
#5903 = CARTESIAN_POINT ( 'NONE',  ( -4.191402346623055664, -90.19547149457073942, 5.607243785695398941 ) ) ;
#5904 = CARTESIAN_POINT ( 'NONE',  ( 50.00000000000000000, -7.999999999999992895, -12.50000000000000178 ) ) ;
#5905 = DIRECTION ( 'NONE',  ( 0.000000000000000000, 1.000000000000000000, 0.000000000000000000 ) ) ;
#5906 = CARTESIAN_POINT ( 'NONE',  ( -1.686450176301617976, -68.29547149457073374, -2.482926158054096000 ) ) ;
#5907 = AXIS2_PLACEMENT_3D ( 'NONE', #5220, #7800, #2033 ) ;
#5908 = AXIS2_PLACEMENT_3D ( 'NONE', #4631, #2625, #5185 ) ;
#5909 = CARTESIAN_POINT ( 'NONE',  ( 1.529537955723688336, -59.85452850542924352, -5.030887037049978971 ) ) ;
#5910 = VERTEX_POINT ( 'NONE', #4156 ) ;
#5911 = CARTESIAN_POINT ( 'NONE',  ( -3.015831842038214639, -78.30452850542926058, -3.989209796945429432 ) ) ;
#5912 = CARTESIAN_POINT ( 'NONE',  ( 6.628020296210689111, -94.09547149457074511, 2.253526892787472757 ) ) ;
#5913 =( NAMED_UNIT ( * ) SI_UNIT ( $, .STERADIAN. ) SOLID_ANGLE_UNIT ( ) );
#5914 = ORIENTED_EDGE ( 'NONE', *, *, #4954, .F. ) ;
#5915 = VECTOR ( 'NONE', #6618, 1000.000000000000000 ) ;
#5916 = CARTESIAN_POINT ( 'NONE',  ( -5.257311121191324155, -72.75452850542924921, 0.09995255151729526277 ) ) ;
#5917 = DIRECTION ( 'NONE',  ( -1.000000000000000000, 0.000000000000000000, 0.000000000000000000 ) ) ;
#5918 = CONTEXT_DEPENDENT_SHAPE_REPRESENTATION ( #827, #5738 ) ;
#5919 = STYLED_ITEM ( 'NONE', ( #2639 ), #7100 ) ;
#5920 = DIRECTION ( 'NONE',  ( 1.000000000000000000, 0.000000000000000000, 0.000000000000000000 ) ) ;
#5921 = CARTESIAN_POINT ( 'NONE',  ( -4.784657899331157260, -80.89547149457074227, 1.454677039711874675 ) ) ;
#5922 = CARTESIAN_POINT ( 'NONE',  ( 1.488389562037239156, -97.00000000000000000, -3.748545376255541850 ) ) ;
#5923 = CARTESIAN_POINT ( 'NONE',  ( -0.8796985632579451542, -59.14547149457074227, -3.030887037049952326 ) ) ;
#5924 = CARTESIAN_POINT ( 'NONE',  ( 6.686770931921523164, -68.10452850542924352, 2.072711028461649008 ) ) ;
#5925 = DIRECTION ( 'NONE',  ( 1.000000000000000000, 0.000000000000000000, 0.000000000000000000 ) ) ;
#5926 = CARTESIAN_POINT ( 'NONE',  ( 0.09506052544075525856, -76.99547149457073658, -4.999999999999997335 ) ) ;
#5927 = CARTESIAN_POINT ( 'NONE',  ( 75.00000000000000000, 80.00000000000000000, -7.500000000000000000 ) ) ;
#5928 = CARTESIAN_POINT ( 'NONE',  ( 4.725907263620340970, -83.40452850542925489, -1.635492904037697981 ) ) ;
#5929 = CARTESIAN_POINT ( 'NONE',  ( 6.686770931921523164, -71.10452850542924352, 2.072711028461649008 ) ) ;
#5930 = CARTESIAN_POINT ( 'NONE',  ( 0.09506052544077665811, -79.99547149457075079, -2.999999999999997780 ) ) ;
#5931 = EDGE_LOOP ( 'NONE', ( #5304, #2804 ) ) ;
#5932 = CARTESIAN_POINT ( 'NONE',  ( 45.19324698792023298, -11.84363253063589205, 2.500000000000000888 ) ) ;
#5933 = CARTESIAN_POINT ( 'NONE',  ( 80.00000000000000000, -19.99999999999999645, -12.50000000000000355 ) ) ;
#5934 = CARTESIAN_POINT ( 'NONE',  ( 1.529537955723691001, -83.85452850542927195, -5.030887037049978971 ) ) ;
#5935 = ORIENTED_EDGE ( 'NONE', *, *, #2729, .T. ) ;
#5936 = CARTESIAN_POINT ( 'NONE',  ( 1.719659006605391172, -79.65452850542925489, 4.969112962950015699 ) ) ;
#5937 = CARTESIAN_POINT ( 'NONE',  ( -2.882544866740855749, -89.89547149457074227, 0.8366430509619596778 ) ) ;
#5938 = CARTESIAN_POINT ( 'NONE',  ( 0.000000000000000000, 0.000000000000000000, 0.000000000000000000 ) ) ;
#5939 = CARTESIAN_POINT ( 'NONE',  ( 5.257311121191342806, -89.25452850542924921, -0.09995255151729465215 ) ) ;
#5940 = CARTESIAN_POINT ( 'NONE',  ( 2.369498399071075401, -61.84547149457074511, -6.969112962950057444 ) ) ;
#5941 = CARTESIAN_POINT ( 'NONE',  ( 2.882544866740895717, -68.10452850542924352, 0.8366430509618999478 ) ) ;
#5942 = EDGE_CURVE ( 'NONE', #4020, #5889, #791, .T. ) ;
#5943 = ADVANCED_FACE ( 'NONE', ( #160 ), #4704, .F. ) ;
#5944 = DIRECTION ( 'NONE',  ( 0.000000000000000000, -3.469446951953615175E-16, -1.000000000000000000 ) ) ;
#5945 = DIRECTION ( 'NONE',  ( 1.000000000000000000, 0.000000000000000000, 0.000000000000000000 ) ) ;
#5946 = CARTESIAN_POINT ( 'NONE',  ( 2.493201789345272257, -80.55452850542926058, -1.934965279058294518 ) ) ;
#5947 = CARTESIAN_POINT ( 'NONE',  ( 4.191402346623198660, -85.80452850542926058, 5.607243785695311900 ) ) ;
#5948 = CARTESIAN_POINT ( 'NONE',  ( 54.99999999999999289, 80.00000000000000000, 7.500000000000000000 ) ) ;
#5949 = CARTESIAN_POINT ( 'NONE',  ( -2.369498399071054529, -93.34547149457073090, 6.969112962950058332 ) ) ;
#5950 = FACE_OUTER_BOUND ( 'NONE', #7464, .T. ) ;
#5951 = PLANE ( 'NONE',  #6495 ) ;
#5952 = CARTESIAN_POINT ( 'NONE',  ( -1.686450176301617976, -71.29547149457074795, -2.482926158054096000 ) ) ;
#5953 = CARTESIAN_POINT ( 'NONE',  ( -1.719659006605374962, -57.15452850542924068, -4.969112962950016588 ) ) ;
#5954 = ORIENTED_EDGE ( 'NONE', *, *, #438, .F. ) ;
#5955 = CARTESIAN_POINT ( 'NONE',  ( -4.784657899331191011, -69.60452850542925773, -1.454677039711773867 ) ) ;
#5956 = CARTESIAN_POINT ( 'NONE',  ( -6.628020296210666018, -83.59547149457075932, -2.253526892787471869 ) ) ;
#5957 = ORIENTED_EDGE ( 'NONE', *, *, #4049, .F. ) ;
#5958 = CARTESIAN_POINT ( 'NONE',  ( 4.312004677471076519, -79.95452850542922363, 3.009306630940844496 ) ) ;
#5959 = FACE_OUTER_BOUND ( 'NONE', #3788, .T. ) ;
#5960 =( BOUNDED_SURFACE ( )  B_SPLINE_SURFACE ( 3, 2, ( 
 ( #7840, #834, #161, #4040, #6607, #7283, #3996, #5846, #240, #1343, #2740, #4619, #5978, #2657, #4663, #4077, #5302, #5340, #7885, #202, #7160, #2109, #2781, #5384, #3914, #1509, #6482, #3287, #6180, #1552, #1636, #3488, #7491, #1042, #4833, #4157, #8126, #3612, #7411, #6095, #4196, #4116, #2901, #6058, #2314, #1592, #3021, #6221, #1001, #5506, #8087, #5583, #405, #322, #4878, #8164, #3567, #283, #1719, #4278, #2860, #5466, #6137, #6685, #916, #6728, #6851, #958, #2392, #1082, #3652, #7326, #5423, #7449, #3527, #8005, #7362, #2233, #5545, #2272, #4789, #1680, #8045, #4919, #6766, #362, #2939, #4240, #6808, #2979, #2357, #444, #6305, #4439, #4396, #7655, #1889, #5743, #5037, #1121, #4480, #4952, #1209, #3735, #7019, #3696, #8283, #7695, #2474, #606, #3779, #1246, #8202, #526, #6974, #1927, #1287, #3817, #5911, #6266, #6389, #7530, #7611, #484, #5118, #3188, #1846, #1803, #8324, #2557, #6349, #3105, #567, #1761, #5661, #3061, #2512, #7567, #770, #3857, #3145, #5702, #5076, #3350, #7060, #8242, #6427, #141, #4316, #5621, #6887, #2433, #4995, #4359, #6933, #1167, #4644, #5323, #8030, #2130, #5404, #2764, #4102, #7264, #2089, #182, #2802, #1491, #7906, #4682, #2257, #4772, #4059, #1575, #6627, #3473, #5955, #4813, #6589, #7390, #983, #4181, #2172, #3397, #855, #6751, #817, #1619, #3436, #5363, #4725, #7306, #5998, #223, #1448, #6039, #2214, #7947, #7348, #1531, #7986, #4141, #3513, #6669, #7226, #3550, #2722, #900, #263, #6709, #4018, #2845, #5451, #941, #6081, #306, #2883, #6121, #5280, #7862, #5647, #5018, #3045, #1190, #1661, #7553, #2924, #3001, #4860, #506, #2415, #6203, #5529, #1150, #4978, #427, #7475, #5567, #5489, #4260, #7432, #3676, #2964, #4382, #7594, #2377, #6874, #1103, #6957, #1784, #1704, #6247, #3760, #4939, #4221, #3084, #8226, #6794, #6832, #7513, #8069 ),
 ( #469, #1025, #3592, #2456, #8109, #8150, #6917, #3720, #1829, #6162, #385, #6290, #5606, #1064, #1743, #2336, #345, #4302, #8187, #4340, #2299, #4903, #3638, #3883, #1356, #3801, #4462, #4418, #7042, #1312, #7171, #5187, #5684, #1273, #4506, #7001, #3301, #6454, #2669, #3212, #3171, #7809, #3926, #7085, #40, #86, #5100, #7765, #2537, #1871, #676, #3256, #2040, #2579, #1230, #5140, #3128, #8267, #592, #5857, #5726, #5811, #6371, #7720, #7679, #2498, #8304, #6411, #1911, #3842, #629, #5226, #2628, #5770, #1996, #8337, #4546, #1956, #4588, #7129, #1395, #6333, #551, #6493, #715, #5059, #7637, #7852, #296, #2752, #4051, #5990, #213, #4674, #5313, #2713, #7296, #2247, #3502, #2873, #4802, #2078, #4091, #5946, #5271, #4008, #6537, #2203, #7254, #131, #1523, #7377, #1564, #4633, #2793, #7216, #759, #1440, #6577, #6029, #3464, #7896, #253, #3425, #6661, #890, #4758, #6619, #808, #6072, #3968, #5353, #2121, #2835, #3388, #5396, #6698, #1483, #7977, #7936, #7339, #172, #846, #2163, #929, #5439, #4130, #3341, #4716, #8020, #5899, #4252, #6110, #1774, #3666, #7466, #6784, #2407, #6234, #1695, #377, #6822, #4171, #5521, #336, #4932, #4210, #5638, #498, #3626, #8141, #2369, #8219, #460, #2953, #7505, #2447, #6193, #2913, #4329, #6903, #5480, #8102, #7425, #1055, #6151, #1016, #1651, #1141, #3034, #2328, #5596, #3584, #1735, #4849, #3710, #8059, #6280, #5009, #3076, #419, #2286, #4891, #1606, #2992, #6742, #5558, #4292, #6864, #1094, #8178, #4968, #7544, #972, #3540, #7119, #3918, #78, #3120, #7712, #1224, #542, #7627, #1821, #5803, #2528, #3749, #5133, #2661, #5177, #6323, #6404, #5675, #4373, #8257, #1862, #1304, #7077, #582, #3874, #7034, #1945, #4498, #32, #7671, #2491, #1347, #7582, #3834, #6365, #6443, #5052, #2572, #1988, #5091, #3247, #622, #664, #4410, #3164, #1262 ),
 ( #6992, #7756, #2615, #1904, #3793, #4538, #6486, #4453, #5719, #3203, #6948, #8298, #5759, #707, #4293, #3291, #5850, #1181, #3418, #5982, #3492, #4081, #4000, #206, #6063, #7248, #6530, #5388, #7969, #752, #796, #4044, #2031, #7164, #7844, #2194, #4623, #7929, #5263, #6611, #1433, #4580, #1387, #3958, #2071, #4746, #7208, #2155, #6570, #838, #3378, #3333, #2704, #5306, #5937, #165, #2745, #7330, #7287, #7889, #6653, #2113, #2785, #121, #1556, #5891, #4121, #287, #6689, #4667, #1474, #5344, #920, #4709, #5219, #1513, #882, #3456, #6020, #244, #2824, #7799, #6183, #1125, #2396, #7533, #3699, #6732, #2982, #4837, #4161, #2905, #5427, #1085, #6140, #7367, #409, #6269, #447, #1596, #1683, #963, #8009, #3531, #5470, #4922, #2360, #4200, #7494, #2317, #5549, #8130, #3656, #2942, #6099, #4956, #2864, #7453, #1640, #1723, #326, #4281, #5586, #365, #6854, #4243, #6225, #8049, #6770, #4881, #8167, #1764, #3024, #2237, #2276, #4319, #4793, #5509, #7415, #6892, #1005, #8090, #3571, #6812, #1045, #3615, #7614, #5705, #3064, #4399, #4998, #3821, #3109, #4524, #7741, #2515, #7022, #1249, #7104, #7698, #1849, #6393, #1330, #5079, #1807, #648, #3232, #4362, #6977, #7658, #5625, #7063, #3782, #7570, #609, #3903, #6430, #6936, #1892, #1170, #8206, #3738, #5664, #2560, #8327, #1212, #5121, #8286, #3191, #5746, #1291, #570, #6308, #17, #487, #4442, #6352, #1930, #530, #4483, #5789, #3150, #3860, #2599, #5162, #8245, #1973, #2436, #2478, #5041, #824, #7313, #7784, #5332, #691, #782, #2646, #6636, #193, #3986, #3318, #7274, #2772, #6554, #5246, #3362, #3275, #2058, #5203, #1457, #738, #2181, #5372, #149, #4653, #7234, #4734, #7914, #7830, #4029, #1542, #2731, #2013, #868, #3444, #4565, #4606, #5289, #5835, #63, #5875, #6007, #105, #3404, #6514, #7874, #2689, #7150, #3942, #5923, #7193 ),
 ( #1373, #232, #1417, #2810, #6472, #7955, #2100, #6598, #5965, #2140, #4693, #1500, #4067, #6050, #274, #2853, #5415, #3480, #6678, #7995, #7357, #4782, #4110, #909, #2226, #5662, #445, #4397, #4440, #4996, #6852, #485, #7656, #8203, #6350, #4317, #2980, #2358, #8128, #5546, #3062, #6888, #3106, #3780, #2394, #4920, #6222, #528, #3697, #7531, #7020, #7568, #6267, #6975, #1083, #1805, #7492, #2434, #8243, #5038, #4360, #5623, #1847, #1762, #1720, #6934, #1247, #3819, #4279, #3653, #3022, #568, #1210, #3147, #1168, #2476, #5584, #6390, #6306, #8165, #4953, #8284, #1123, #3736, #5703, #2513, #5077, #7612, #1890, #6552, #6512, #1971, #5833, #15, #7191, #2011, #736, #5201, #689, #6428, #8325, #3316, #3984, #645, #7102, #7061, #1327, #3940, #1455, #7827, #2558, #3901, #7148, #1288, #5921, #4521, #5873, #3230, #2056, #2098, #780, #1371, #2687, #2728, #7739, #4604, #5160, #4481, #103, #5244, #4651, #7781, #3858, #147, #7232, #5744, #6470, #1415, #3273, #3360, #5119, #61, #4563, #5787, #607, #7872, #2597, #5287, #7696, #4027, #2644, #3189, #1928, #2808, #2264, #5962, #1583, #6720, #2138, #2307, #4148, #2770, #5330, #3560, #6005, #4107, #4821, #1629, #6129, #4691, #6634, #4190, #951, #7953, #3478, #230, #7402, #7993, #3520, #2851, #6676, #4065, #191, #6089, #6760, #865, #4732, #7272, #7311, #313, #7442, #5459, #7912, #1540, #4780, #1498, #354, #2179, #2893, #3442, #8037, #8079, #993, #7355, #2931, #5496, #5370, #4870, #907, #6048, #1669, #6596, #822, #5413, #272, #3402, #2224, #1033, #1755, #5030, #3012, #517, #398, #437, #479, #7483, #4232, #3137, #8119, #7604, #3602, #4988, #4912, #5578, #3054, #8158, #8235, #6169, #7562, #6259, #2346, #4310, #559, #1114, #1840, #2387, #6801, #2971, #5536, #1711, #6882, #4947, #4351, #4390, #3646, #4269, #6841, #1796, #7522, #3687, #8277 ),
 ( #6299, #5616, #8195, #3098, #2427, #1074, #6927, #2506, #5068, #6212, #1161, #3729, #6967, #5655, #1199, #2466, #3770, #6342, #5694, #7647, #7774, #5195, #3351, #6464, #2547, #1407, #5912, #7012, #7732, #2679, #639, #6503, #6381, #6420, #684, #5111, #1881, #771, #5734, #5237, #1239, #2638, #7687, #3223, #3264, #5780, #5866, #3809, #2004, #3894, #8317, #1965, #6547, #7094, #7821, #8, #4430, #600, #3181, #1921, #4514, #2587, #4556, #2049, #1281, #4473, #7053, #7141, #5151, #1321, #142, #5820, #54, #96, #3850, #1365, #3934, #728, #3310, #4598, #7182, #3978, #2723, #5281, #7863, #3474, #3551, #346, #4019, #3398, #6590, #307, #6711, #8031, #1532, #7987, #5956, #6122, #2846, #818, #183, #4814, #7265, #5364, #6082, #2884, #7392, #2765, #7907, #5452, #5405, #856, #4726, #1492, #2258, #901, #2215, #4103, #7948, #5324, #7227, #4773, #1620, #2131, #5999, #4683, #224, #7349, #2925, #942, #1449, #2803, #6040, #4060, #4182, #3437, #1576, #6628, #3514, #984, #6752, #264, #4142, #2090, #2173, #4645, #7307, #6670, #1662, #2457, #4904, #3002, #3721, #507, #5019, #1026, #5530, #3087, #3046, #6833, #2378, #7476, #6291, #6875, #5607, #1745, #5568, #2965, #4861, #8188, #5648, #8110, #3639, #3593, #6204, #470, #6334, #4341, #7433, #428, #3677, #6163, #7595, #1065, #2417, #2337, #6918, #6958, #8227, #6248, #7554, #1830, #4261, #1151, #1705, #387, #4979, #1785, #1191, #4303, #8151, #4383, #3762, #2300, #4940, #552, #7514, #5490, #4222, #1104, #8071, #6795, #3129, #2042, #7002, #3927, #8268, #3885, #3802, #7680, #1957, #1912, #7131, #2499, #6455, #5141, #1231, #630, #7810, #1, #6494, #4463, #5685, #5060, #7638, #1872, #3213, #7043, #3257, #717, #2538, #4420, #6372, #677, #3843, #1274, #7172, #7721, #6412, #1357, #593, #4507, #3172, #2580, #5812, #5188, #7086, #5771, #1997, #1313, #5727 ),
 ( #3302, #41, #2629, #5858, #7766, #8305, #5102, #4547, #87, #2670, #5227, #4589, #1397, #3969, #6538, #4009, #6662, #1484, #5314, #4803, #2794, #4052, #4760, #7217, #5354, #132, #5991, #3465, #2836, #7937, #6620, #7978, #7897, #760, #4717, #7379, #1607, #5272, #4634, #7853, #1565, #2204, #930, #2164, #891, #1441, #4172, #4093, #2079, #6578, #6073, #173, #847, #7340, #4131, #297, #809, #3389, #6699, #6030, #2122, #214, #2754, #3503, #7297, #254, #1524, #3427, #5947, #2714, #5397, #2874, #4675, #7255, #5440, #8021, #2248, #3342, #5900, #6111, #1808, #5042, #4957, #3822, #2437, #1213, #4320, #8287, #8329, #4443, #7615, #571, #610, #5627, #5706, #3065, #2397, #4400, #1850, #2561, #3110, #7534, #6394, #5122, #3541, #4363, #7660, #8207, #3151, #2914, #4999, #5665, #1765, #6743, #5747, #6893, #1893, #337, #6979, #1126, #7571, #8246, #6937, #2516, #5587, #3783, #531, #3700, #1171, #3192, #3739, #6310, #973, #2479, #7699, #1931, #8168, #6270, #488, #7023, #5080, #1250, #6353, #4607, #18, #194, #7831, #650, #3233, #1458, #3904, #2015, #2732, #7875, #4031, #2600, #4525, #2101, #2059, #5836, #1374, #6473, #5290, #5876, #7194, #739, #4566, #1974, #3861, #1418, #4654, #7105, #2647, #5163, #5204, #3987, #5333, #3364, #6431, #7785, #2691, #7742, #6599, #64, #6555, #1332, #5924, #5966, #7235, #5247, #783, #825, #3276, #150, #692, #7151, #3405, #2773, #7915, #3319, #3943, #4484, #7064, #1292, #6515, #5790, #106, #6761, #6637, #6679, #6722, #5373, #2141, #1035, #6008, #2934, #7275, #2895, #2811, #910, #953, #3481, #6130, #1501, #5460, #4151, #233, #7997, #6803, #7358, #5498, #6051, #4694, #4068, #869, #3445, #2227, #275, #2267, #8080, #1543, #7956, #2182, #8039, #2854, #5416, #6171, #3522, #4783, #355, #4735, #6090, #7315, #1586, #4823, #4191, #315, #7405, #995, #4111, #1631 ),
 ( #2309, #3562, #4872, #7444, #1672, #4234, #3605, #400, #2973, #5539, #4914, #8121, #3647, #439, #7485, #4271, #1713, #6842, #1075, #2349, #6213, #3013, #2658, #5888, #5800, #4664, #3288, #2068, #5174, #793, #835, #5303, #118, #1430, #1471, #6483, #6567, #3915, #3244, #5260, #2701, #3415, #3955, #29, #7245, #5979, #4495, #5216, #162, #704, #3997, #3871, #5847, #6527, #2612, #7709, #6608, #7753, #2741, #7074, #7841, #1985, #75, #749, #7796, #3375, #1301, #4620, #1384, #4535, #2028, #4041, #4577, #7886, #7161, #1942, #6440, #661, #7116, #3330, #7205, #5934, #2110, #1344, #203, #2782, #2902, #6059, #1553, #1043, #7363, #284, #1002, #3453, #1593, #4706, #2234, #8046, #7412, #4158, #2861, #4197, #4117, #5341, #959, #3613, #6181, #1510, #878, #4078, #6138, #6767, #5507, #6729, #5467, #6017, #406, #323, #6650, #8088, #2315, #241, #917, #3528, #2152, #7284, #7966, #4879, #4743, #2273, #5385, #6096, #6686, #2820, #2191, #5424, #3489, #7327, #8006, #7451, #1637, #4790, #3568, #4834, #363, #2940, #1681, #4241, #6809, #7926, #1280, #7646, #3136, #3686, #5576, #3769, #1237, #6257, #4350, #4309, #6926, #1198, #7052, #5067, #8157, #1160, #4389, #6881, #3179, #1795, #558, #478, #1879, #7686, #3808, #6966, #8276, #8316, #4987, #4427, #2425, #1753, #6340, #5693, #1920, #2465, #1113, #5733, #4471, #3010, #3728, #7011, #7561, #2505, #2386, #6298, #5029, #3053, #6211, #5109, #5615, #6380, #4946, #599, #8194, #516, #7603, #3096, #2546, #7521, #436, #8234, #5654, #1839, #179, #727, #7224, #5194, #3849, #3222, #638, #6419, #3933, #7772, #3977, #4642, #3263, #5778, #7092, #1406, #4554, #53, #7904, #5864, #7139, #7860, #1964, #95, #7, #3308, #6545, #5909, #2678, #1364, #2720, #2636, #2586, #1319, #6501, #2003, #6463, #3893, #3395, #139, #5236, #5278, #5819, #4597, #683, #5953, #7730 ) ),
 .UNSPECIFIED., .T., .F., .T. ) 
 B_SPLINE_SURFACE_WITH_KNOTS ( ( 4, 3, 4 ),
 ( 3, 2, 2, 2, 2, 2, 2, 2, 2, 2, 2, 2, 2, 2, 2, 2, 2, 2, 2, 2, 2, 2, 2, 2, 2, 2, 2, 2, 2, 2, 2, 2, 2, 2, 2, 2, 2, 2, 2, 2, 2, 2, 2, 2, 2, 2, 2, 2, 2, 2, 2, 2, 2, 2, 2, 2, 2, 2, 2, 2, 2, 2, 2, 2, 2, 2, 2, 2, 2, 2, 2, 2, 2, 2, 2, 2, 2, 2, 2, 2, 2, 2, 2, 2, 2, 2, 2, 2, 2, 2, 2, 2, 2, 2, 2, 2, 2, 2, 2, 2, 2, 2, 2, 2, 2, 2, 2, 2, 2, 2, 2, 2, 2, 2, 2, 2, 2, 2, 2, 2, 2, 2, 2, 2, 2, 2, 2, 2, 2, 2, 3 ),
 ( 0.000000000000000000, 0.5000000000000000000, 1.000000000000000000 ),
 ( 0.000000000000000000, 0.007692307692307692735, 0.01538461538461538547, 0.02307692307692307820, 0.03076923076923077094, 0.03846153846153846367, 0.04615384615384615641, 0.05384615384615384914, 0.06153846153846154188, 0.06923076923076923461, 0.07692307692307692735, 0.08461538461538462008, 0.09230769230769231282, 0.1000000000000000056, 0.1076923076923076983, 0.1153846153846153910, 0.1230769230769230838, 0.1307692307692307765, 0.1384615384615384692, 0.1461538461538461620, 0.1538461538461538547, 0.1615384615384615474, 0.1692307692307692402, 0.1769230769230769329, 0.1846153846153846256, 0.1923076923076923184, 0.2000000000000000111, 0.2076923076923077038, 0.2153846153846153966, 0.2230769230769230893, 0.2307692307692307820, 0.2384615384615384748, 0.2461538461538461675, 0.2538461538461538325, 0.2615384615384615530, 0.2692307692307692180, 0.2769230769230769384, 0.2846153846153846034, 0.2923076923076923239, 0.2999999999999999889, 0.3076923076923077094, 0.3153846153846153744, 0.3230769230769230949, 0.3307692307692307598, 0.3384615384615384803, 0.3461538461538461453, 0.3538461538461538658, 0.3615384615384615308, 0.3692307692307692513, 0.3769230769230769162, 0.3846153846153846367, 0.3923076923076923017, 0.4000000000000000222, 0.4076923076923076872, 0.4153846153846154077, 0.4230769230769230727, 0.4307692307692307931, 0.4384615384615384581, 0.4461538461538461786, 0.4538461538461538436, 0.4615384615384615641, 0.4692307692307692291, 0.4769230769230769496, 0.4846153846153846145, 0.4923076923076923350, 0.5000000000000000000, 0.5076923076923076650, 0.5153846153846153300, 0.5230769230769231060, 0.5307692307692307709, 0.5384615384615384359, 0.5461538461538461009, 0.5538461538461538769, 0.5615384615384615419, 0.5692307692307692069, 0.5769230769230768718, 0.5846153846153846478, 0.5923076923076923128, 0.5999999999999999778, 0.6076923076923076428, 0.6153846153846154188, 0.6230769230769230838, 0.6307692307692307487, 0.6384615384615384137, 0.6461538461538461897, 0.6538461538461538547, 0.6615384615384615197, 0.6692307692307691847, 0.6769230769230769607, 0.6846153846153846256, 0.6923076923076922906, 0.6999999999999999556, 0.7076923076923077316, 0.7153846153846153966, 0.7230769230769230616, 0.7307692307692307265, 0.7384615384615385025, 0.7461538461538461675, 0.7538461538461538325, 0.7615384615384614975, 0.7692307692307692735, 0.7769230769230769384, 0.7846153846153846034, 0.7923076923076922684, 0.8000000000000000444, 0.8076923076923077094, 0.8153846153846153744, 0.8230769230769230393, 0.8307692307692308153, 0.8384615384615384803, 0.8461538461538461453, 0.8538461538461538103, 0.8615384615384615863, 0.8692307692307692513, 0.8769230769230769162, 0.8846153846153845812, 0.8923076923076923572, 0.9000000000000000222, 0.9076923076923076872, 0.9153846153846153522, 0.9230769230769231282, 0.9307692307692307931, 0.9384615384615384581, 0.9461538461538461231, 0.9538461538461538991, 0.9615384615384615641, 0.9692307692307692291, 0.9769230769230768940, 0.9846153846153846700, 0.9923076923076923350, 1.000000000000000000 ),
 .UNSPECIFIED. ) 
 GEOMETRIC_REPRESENTATION_ITEM ( )  RATIONAL_B_SPLINE_SURFACE ( (
 ( 1.000000000000000000, 0.9510565162951535312, 1.000000000000000000, 0.9510565162951535312, 1.000000000000000000, 0.9510565162951535312, 1.000000000000000000, 0.9510565162951535312, 1.000000000000000000, 0.9510565162951535312, 1.000000000000000000, 0.9510565162951535312, 1.000000000000000000, 0.9510565162951535312, 1.000000000000000000, 0.9510565162951535312, 1.000000000000000000, 0.9510565162951535312, 1.000000000000000000, 0.9510565162951535312, 1.000000000000000000, 0.9510565162951535312, 1.000000000000000000, 0.9510565162951535312, 1.000000000000000000, 0.9510565162951535312, 1.000000000000000000, 0.9510565162951535312, 1.000000000000000000, 0.9510565162951535312, 1.000000000000000000, 0.9510565162951535312, 1.000000000000000000, 0.9510565162951535312, 1.000000000000000000, 0.9510565162951535312, 1.000000000000000000, 0.9510565162951535312, 1.000000000000000000, 0.9510565162951535312, 1.000000000000000000, 0.9510565162951535312, 1.000000000000000000, 0.9510565162951535312, 1.000000000000000000, 0.9510565162951535312, 1.000000000000000000, 0.9510565162951535312, 1.000000000000000000, 0.9510565162951535312, 1.000000000000000000, 0.9510565162951535312, 1.000000000000000000, 0.9510565162951535312, 1.000000000000000000, 0.9510565162951535312, 1.000000000000000000, 0.9510565162951535312, 1.000000000000000000, 0.9510565162951535312, 1.000000000000000000, 0.9510565162951535312, 1.000000000000000000, 0.9510565162951535312, 1.000000000000000000, 0.9510565162951535312, 1.000000000000000000, 0.9510565162951535312, 1.000000000000000000, 0.9510565162951535312, 1.000000000000000000, 0.9510565162951535312, 1.000000000000000000, 0.9510565162951535312, 1.000000000000000000, 0.9510565162951535312, 1.000000000000000000, 0.9510565162951535312, 1.000000000000000000, 0.9510565162951535312, 1.000000000000000000, 0.9510565162951535312, 1.000000000000000000, 0.9510565162951535312, 1.000000000000000000, 0.9510565162951535312, 1.000000000000000000, 0.9510565162951535312, 1.000000000000000000, 0.9510565162951535312, 1.000000000000000000, 0.9510565162951535312, 1.000000000000000000, 0.9510565162951535312, 1.000000000000000000, 0.9510565162951535312, 1.000000000000000000, 0.9510565162951535312, 1.000000000000000000, 0.9510565162951535312, 1.000000000000000000, 0.9510565162951535312, 1.000000000000000000, 0.9510565162951535312, 1.000000000000000000, 0.9510565162951535312, 1.000000000000000000, 0.9510565162951535312, 1.000000000000000000, 0.9510565162951535312, 1.000000000000000000, 0.9510565162951535312, 1.000000000000000000, 0.9510565162951535312, 1.000000000000000000, 0.9510565162951535312, 1.000000000000000000, 0.9510565162951535312, 1.000000000000000000, 0.9510565162951535312, 1.000000000000000000, 0.9510565162951535312, 1.000000000000000000, 0.9510565162951535312, 1.000000000000000000, 0.9510565162951535312, 1.000000000000000000, 0.9510565162951535312, 1.000000000000000000, 0.9510565162951535312, 1.000000000000000000, 0.9510565162951535312, 1.000000000000000000, 0.9510565162951535312, 1.000000000000000000, 0.9510565162951535312, 1.000000000000000000, 0.9510565162951535312, 1.000000000000000000, 0.9510565162951535312, 1.000000000000000000, 0.9510565162951535312, 1.000000000000000000, 0.9510565162951535312, 1.000000000000000000, 0.9510565162951535312, 1.000000000000000000, 0.9510565162951535312, 1.000000000000000000, 0.9510565162951535312, 1.000000000000000000, 0.9510565162951535312, 1.000000000000000000, 0.9510565162951535312, 1.000000000000000000, 0.9510565162951535312, 1.000000000000000000, 0.9510565162951535312, 1.000000000000000000, 0.9510565162951535312, 1.000000000000000000, 0.9510565162951535312, 1.000000000000000000, 0.9510565162951535312, 1.000000000000000000, 0.9510565162951535312, 1.000000000000000000, 0.9510565162951535312, 1.000000000000000000, 0.9510565162951535312, 1.000000000000000000, 0.9510565162951535312, 1.000000000000000000, 0.9510565162951535312, 1.000000000000000000, 0.9510565162951535312, 1.000000000000000000, 0.9510565162951535312, 1.000000000000000000, 0.9510565162951535312, 1.000000000000000000, 0.9510565162951535312, 1.000000000000000000, 0.9510565162951535312, 1.000000000000000000, 0.9510565162951535312, 1.000000000000000000, 0.9510565162951535312, 1.000000000000000000, 0.9510565162951535312, 1.000000000000000000, 0.9510565162951535312, 1.000000000000000000, 0.9510565162951535312, 1.000000000000000000, 0.9510565162951535312, 1.000000000000000000, 0.9510565162951535312, 1.000000000000000000, 0.9510565162951535312, 1.000000000000000000, 0.9510565162951535312, 1.000000000000000000, 0.9510565162951535312, 1.000000000000000000, 0.9510565162951535312, 1.000000000000000000, 0.9510565162951535312, 1.000000000000000000, 0.9510565162951535312, 1.000000000000000000, 0.9510565162951535312, 1.000000000000000000, 0.9510565162951535312, 1.000000000000000000, 0.9510565162951535312, 1.000000000000000000, 0.9510565162951535312, 1.000000000000000000, 0.9510565162951535312, 1.000000000000000000, 0.9510565162951535312, 1.000000000000000000, 0.9510565162951535312, 1.000000000000000000, 0.9510565162951535312, 1.000000000000000000, 0.9510565162951535312, 1.000000000000000000, 0.9510565162951535312, 1.000000000000000000, 0.9510565162951535312, 1.000000000000000000, 0.9510565162951535312, 1.000000000000000000, 0.9510565162951535312, 1.000000000000000000, 0.9510565162951535312, 1.000000000000000000, 0.9510565162951535312, 1.000000000000000000, 0.9510565162951535312, 1.000000000000000000, 0.9510565162951535312, 1.000000000000000000, 0.9510565162951535312, 1.000000000000000000, 0.9510565162951535312, 1.000000000000000000, 0.9510565162951535312, 1.000000000000000000, 0.9510565162951535312, 1.000000000000000000, 0.9510565162951535312, 1.000000000000000000, 0.9510565162951535312, 1.000000000000000000, 0.9510565162951535312, 1.000000000000000000, 0.9510565162951535312, 1.000000000000000000),
 ( 0.3333333333333333703, 0.3170188387650512141, 0.3333333333333333703, 0.3170188387650512141, 0.3333333333333333703, 0.3170188387650512141, 0.3333333333333333703, 0.3170188387650512141, 0.3333333333333333703, 0.3170188387650512141, 0.3333333333333333703, 0.3170188387650512141, 0.3333333333333333703, 0.3170188387650512141, 0.3333333333333333703, 0.3170188387650512141, 0.3333333333333333703, 0.3170188387650512141, 0.3333333333333333703, 0.3170188387650512141, 0.3333333333333333703, 0.3170188387650512141, 0.3333333333333333703, 0.3170188387650512141, 0.3333333333333333703, 0.3170188387650512141, 0.3333333333333333703, 0.3170188387650512141, 0.3333333333333333703, 0.3170188387650512141, 0.3333333333333333703, 0.3170188387650512141, 0.3333333333333333703, 0.3170188387650512141, 0.3333333333333333703, 0.3170188387650512141, 0.3333333333333333703, 0.3170188387650512141, 0.3333333333333333703, 0.3170188387650512141, 0.3333333333333333703, 0.3170188387650512141, 0.3333333333333333703, 0.3170188387650512141, 0.3333333333333333703, 0.3170188387650512141, 0.3333333333333333703, 0.3170188387650512141, 0.3333333333333333703, 0.3170188387650512141, 0.3333333333333333703, 0.3170188387650512141, 0.3333333333333333703, 0.3170188387650512141, 0.3333333333333333703, 0.3170188387650512141, 0.3333333333333333703, 0.3170188387650512141, 0.3333333333333333703, 0.3170188387650512141, 0.3333333333333333703, 0.3170188387650512141, 0.3333333333333333703, 0.3170188387650512141, 0.3333333333333333703, 0.3170188387650512141, 0.3333333333333333703, 0.3170188387650512141, 0.3333333333333333703, 0.3170188387650512141, 0.3333333333333333703, 0.3170188387650512141, 0.3333333333333333703, 0.3170188387650512141, 0.3333333333333333703, 0.3170188387650512141, 0.3333333333333333703, 0.3170188387650512141, 0.3333333333333333703, 0.3170188387650512141, 0.3333333333333333703, 0.3170188387650512141, 0.3333333333333333703, 0.3170188387650512141, 0.3333333333333333703, 0.3170188387650512141, 0.3333333333333333703, 0.3170188387650512141, 0.3333333333333333703, 0.3170188387650512141, 0.3333333333333333703, 0.3170188387650512141, 0.3333333333333333703, 0.3170188387650512141, 0.3333333333333333703, 0.3170188387650512141, 0.3333333333333333703, 0.3170188387650512141, 0.3333333333333333703, 0.3170188387650512141, 0.3333333333333333703, 0.3170188387650512141, 0.3333333333333333703, 0.3170188387650512141, 0.3333333333333333703, 0.3170188387650512141, 0.3333333333333333703, 0.3170188387650512141, 0.3333333333333333703, 0.3170188387650512141, 0.3333333333333333703, 0.3170188387650512141, 0.3333333333333333703, 0.3170188387650512141, 0.3333333333333333703, 0.3170188387650512141, 0.3333333333333333703, 0.3170188387650512141, 0.3333333333333333703, 0.3170188387650512141, 0.3333333333333333703, 0.3170188387650512141, 0.3333333333333333703, 0.3170188387650512141, 0.3333333333333333703, 0.3170188387650512141, 0.3333333333333333703, 0.3170188387650512141, 0.3333333333333333703, 0.3170188387650512141, 0.3333333333333333703, 0.3170188387650512141, 0.3333333333333333703, 0.3170188387650512141, 0.3333333333333333703, 0.3170188387650512141, 0.3333333333333333703, 0.3170188387650512141, 0.3333333333333333703, 0.3170188387650512141, 0.3333333333333333703, 0.3170188387650512141, 0.3333333333333333703, 0.3170188387650512141, 0.3333333333333333703, 0.3170188387650512141, 0.3333333333333333703, 0.3170188387650512141, 0.3333333333333333703, 0.3170188387650512141, 0.3333333333333333703, 0.3170188387650512141, 0.3333333333333333703, 0.3170188387650512141, 0.3333333333333333703, 0.3170188387650512141, 0.3333333333333333703, 0.3170188387650512141, 0.3333333333333333703, 0.3170188387650512141, 0.3333333333333333703, 0.3170188387650512141, 0.3333333333333333703, 0.3170188387650512141, 0.3333333333333333703, 0.3170188387650512141, 0.3333333333333333703, 0.3170188387650512141, 0.3333333333333333703, 0.3170188387650512141, 0.3333333333333333703, 0.3170188387650512141, 0.3333333333333333703, 0.3170188387650512141, 0.3333333333333333703, 0.3170188387650512141, 0.3333333333333333703, 0.3170188387650512141, 0.3333333333333333703, 0.3170188387650512141, 0.3333333333333333703, 0.3170188387650512141, 0.3333333333333333703, 0.3170188387650512141, 0.3333333333333333703, 0.3170188387650512141, 0.3333333333333333703, 0.3170188387650512141, 0.3333333333333333703, 0.3170188387650512141, 0.3333333333333333703, 0.3170188387650512141, 0.3333333333333333703, 0.3170188387650512141, 0.3333333333333333703, 0.3170188387650512141, 0.3333333333333333703, 0.3170188387650512141, 0.3333333333333333703, 0.3170188387650512141, 0.3333333333333333703, 0.3170188387650512141, 0.3333333333333333703, 0.3170188387650512141, 0.3333333333333333703, 0.3170188387650512141, 0.3333333333333333703, 0.3170188387650512141, 0.3333333333333333703, 0.3170188387650512141, 0.3333333333333333703, 0.3170188387650512141, 0.3333333333333333703, 0.3170188387650512141, 0.3333333333333333703, 0.3170188387650512141, 0.3333333333333333703, 0.3170188387650512141, 0.3333333333333333703, 0.3170188387650512141, 0.3333333333333333703, 0.3170188387650512141, 0.3333333333333333703, 0.3170188387650512141, 0.3333333333333333703, 0.3170188387650512141, 0.3333333333333333703, 0.3170188387650512141, 0.3333333333333333703, 0.3170188387650512141, 0.3333333333333333703, 0.3170188387650512141, 0.3333333333333333703, 0.3170188387650512141, 0.3333333333333333703, 0.3170188387650512141, 0.3333333333333333703, 0.3170188387650512141, 0.3333333333333333703, 0.3170188387650512141, 0.3333333333333333703, 0.3170188387650512141, 0.3333333333333333703, 0.3170188387650512141, 0.3333333333333333703, 0.3170188387650512141, 0.3333333333333333703, 0.3170188387650512141, 0.3333333333333333703, 0.3170188387650512141, 0.3333333333333333703, 0.3170188387650512141, 0.3333333333333333703, 0.3170188387650512141, 0.3333333333333333703, 0.3170188387650512141, 0.3333333333333333703, 0.3170188387650512141, 0.3333333333333333703, 0.3170188387650512141, 0.3333333333333333703),
 ( 0.3333333333333333703, 0.3170188387650512141, 0.3333333333333333703, 0.3170188387650512141, 0.3333333333333333703, 0.3170188387650512141, 0.3333333333333333703, 0.3170188387650512141, 0.3333333333333333703, 0.3170188387650512141, 0.3333333333333333703, 0.3170188387650512141, 0.3333333333333333703, 0.3170188387650512141, 0.3333333333333333703, 0.3170188387650512141, 0.3333333333333333703, 0.3170188387650512141, 0.3333333333333333703, 0.3170188387650512141, 0.3333333333333333703, 0.3170188387650512141, 0.3333333333333333703, 0.3170188387650512141, 0.3333333333333333703, 0.3170188387650512141, 0.3333333333333333703, 0.3170188387650512141, 0.3333333333333333703, 0.3170188387650512141, 0.3333333333333333703, 0.3170188387650512141, 0.3333333333333333703, 0.3170188387650512141, 0.3333333333333333703, 0.3170188387650512141, 0.3333333333333333703, 0.3170188387650512141, 0.3333333333333333703, 0.3170188387650512141, 0.3333333333333333703, 0.3170188387650512141, 0.3333333333333333703, 0.3170188387650512141, 0.3333333333333333703, 0.3170188387650512141, 0.3333333333333333703, 0.3170188387650512141, 0.3333333333333333703, 0.3170188387650512141, 0.3333333333333333703, 0.3170188387650512141, 0.3333333333333333703, 0.3170188387650512141, 0.3333333333333333703, 0.3170188387650512141, 0.3333333333333333703, 0.3170188387650512141, 0.3333333333333333703, 0.3170188387650512141, 0.3333333333333333703, 0.3170188387650512141, 0.3333333333333333703, 0.3170188387650512141, 0.3333333333333333703, 0.3170188387650512141, 0.3333333333333333703, 0.3170188387650512141, 0.3333333333333333703, 0.3170188387650512141, 0.3333333333333333703, 0.3170188387650512141, 0.3333333333333333703, 0.3170188387650512141, 0.3333333333333333703, 0.3170188387650512141, 0.3333333333333333703, 0.3170188387650512141, 0.3333333333333333703, 0.3170188387650512141, 0.3333333333333333703, 0.3170188387650512141, 0.3333333333333333703, 0.3170188387650512141, 0.3333333333333333703, 0.3170188387650512141, 0.3333333333333333703, 0.3170188387650512141, 0.3333333333333333703, 0.3170188387650512141, 0.3333333333333333703, 0.3170188387650512141, 0.3333333333333333703, 0.3170188387650512141, 0.3333333333333333703, 0.3170188387650512141, 0.3333333333333333703, 0.3170188387650512141, 0.3333333333333333703, 0.3170188387650512141, 0.3333333333333333703, 0.3170188387650512141, 0.3333333333333333703, 0.3170188387650512141, 0.3333333333333333703, 0.3170188387650512141, 0.3333333333333333703, 0.3170188387650512141, 0.3333333333333333703, 0.3170188387650512141, 0.3333333333333333703, 0.3170188387650512141, 0.3333333333333333703, 0.3170188387650512141, 0.3333333333333333703, 0.3170188387650512141, 0.3333333333333333703, 0.3170188387650512141, 0.3333333333333333703, 0.3170188387650512141, 0.3333333333333333703, 0.3170188387650512141, 0.3333333333333333703, 0.3170188387650512141, 0.3333333333333333703, 0.3170188387650512141, 0.3333333333333333703, 0.3170188387650512141, 0.3333333333333333703, 0.3170188387650512141, 0.3333333333333333703, 0.3170188387650512141, 0.3333333333333333703, 0.3170188387650512141, 0.3333333333333333703, 0.3170188387650512141, 0.3333333333333333703, 0.3170188387650512141, 0.3333333333333333703, 0.3170188387650512141, 0.3333333333333333703, 0.3170188387650512141, 0.3333333333333333703, 0.3170188387650512141, 0.3333333333333333703, 0.3170188387650512141, 0.3333333333333333703, 0.3170188387650512141, 0.3333333333333333703, 0.3170188387650512141, 0.3333333333333333703, 0.3170188387650512141, 0.3333333333333333703, 0.3170188387650512141, 0.3333333333333333703, 0.3170188387650512141, 0.3333333333333333703, 0.3170188387650512141, 0.3333333333333333703, 0.3170188387650512141, 0.3333333333333333703, 0.3170188387650512141, 0.3333333333333333703, 0.3170188387650512141, 0.3333333333333333703, 0.3170188387650512141, 0.3333333333333333703, 0.3170188387650512141, 0.3333333333333333703, 0.3170188387650512141, 0.3333333333333333703, 0.3170188387650512141, 0.3333333333333333703, 0.3170188387650512141, 0.3333333333333333703, 0.3170188387650512141, 0.3333333333333333703, 0.3170188387650512141, 0.3333333333333333703, 0.3170188387650512141, 0.3333333333333333703, 0.3170188387650512141, 0.3333333333333333703, 0.3170188387650512141, 0.3333333333333333703, 0.3170188387650512141, 0.3333333333333333703, 0.3170188387650512141, 0.3333333333333333703, 0.3170188387650512141, 0.3333333333333333703, 0.3170188387650512141, 0.3333333333333333703, 0.3170188387650512141, 0.3333333333333333703, 0.3170188387650512141, 0.3333333333333333703, 0.3170188387650512141, 0.3333333333333333703, 0.3170188387650512141, 0.3333333333333333703, 0.3170188387650512141, 0.3333333333333333703, 0.3170188387650512141, 0.3333333333333333703, 0.3170188387650512141, 0.3333333333333333703, 0.3170188387650512141, 0.3333333333333333703, 0.3170188387650512141, 0.3333333333333333703, 0.3170188387650512141, 0.3333333333333333703, 0.3170188387650512141, 0.3333333333333333703, 0.3170188387650512141, 0.3333333333333333703, 0.3170188387650512141, 0.3333333333333333703, 0.3170188387650512141, 0.3333333333333333703, 0.3170188387650512141, 0.3333333333333333703, 0.3170188387650512141, 0.3333333333333333703, 0.3170188387650512141, 0.3333333333333333703, 0.3170188387650512141, 0.3333333333333333703, 0.3170188387650512141, 0.3333333333333333703, 0.3170188387650512141, 0.3333333333333333703, 0.3170188387650512141, 0.3333333333333333703, 0.3170188387650512141, 0.3333333333333333703, 0.3170188387650512141, 0.3333333333333333703, 0.3170188387650512141, 0.3333333333333333703, 0.3170188387650512141, 0.3333333333333333703, 0.3170188387650512141, 0.3333333333333333703, 0.3170188387650512141, 0.3333333333333333703, 0.3170188387650512141, 0.3333333333333333703, 0.3170188387650512141, 0.3333333333333333703, 0.3170188387650512141, 0.3333333333333333703, 0.3170188387650512141, 0.3333333333333333703, 0.3170188387650512141, 0.3333333333333333703, 0.3170188387650512141, 0.3333333333333333703, 0.3170188387650512141, 0.3333333333333333703),
 ( 1.000000000000000000, 0.9510565162951535312, 1.000000000000000000, 0.9510565162951535312, 1.000000000000000000, 0.9510565162951535312, 1.000000000000000000, 0.9510565162951535312, 1.000000000000000000, 0.9510565162951535312, 1.000000000000000000, 0.9510565162951535312, 1.000000000000000000, 0.9510565162951535312, 1.000000000000000000, 0.9510565162951535312, 1.000000000000000000, 0.9510565162951535312, 1.000000000000000000, 0.9510565162951535312, 1.000000000000000000, 0.9510565162951535312, 1.000000000000000000, 0.9510565162951535312, 1.000000000000000000, 0.9510565162951535312, 1.000000000000000000, 0.9510565162951535312, 1.000000000000000000, 0.9510565162951535312, 1.000000000000000000, 0.9510565162951535312, 1.000000000000000000, 0.9510565162951535312, 1.000000000000000000, 0.9510565162951535312, 1.000000000000000000, 0.9510565162951535312, 1.000000000000000000, 0.9510565162951535312, 1.000000000000000000, 0.9510565162951535312, 1.000000000000000000, 0.9510565162951535312, 1.000000000000000000, 0.9510565162951535312, 1.000000000000000000, 0.9510565162951535312, 1.000000000000000000, 0.9510565162951535312, 1.000000000000000000, 0.9510565162951535312, 1.000000000000000000, 0.9510565162951535312, 1.000000000000000000, 0.9510565162951535312, 1.000000000000000000, 0.9510565162951535312, 1.000000000000000000, 0.9510565162951535312, 1.000000000000000000, 0.9510565162951535312, 1.000000000000000000, 0.9510565162951535312, 1.000000000000000000, 0.9510565162951535312, 1.000000000000000000, 0.9510565162951535312, 1.000000000000000000, 0.9510565162951535312, 1.000000000000000000, 0.9510565162951535312, 1.000000000000000000, 0.9510565162951535312, 1.000000000000000000, 0.9510565162951535312, 1.000000000000000000, 0.9510565162951535312, 1.000000000000000000, 0.9510565162951535312, 1.000000000000000000, 0.9510565162951535312, 1.000000000000000000, 0.9510565162951535312, 1.000000000000000000, 0.9510565162951535312, 1.000000000000000000, 0.9510565162951535312, 1.000000000000000000, 0.9510565162951535312, 1.000000000000000000, 0.9510565162951535312, 1.000000000000000000, 0.9510565162951535312, 1.000000000000000000, 0.9510565162951535312, 1.000000000000000000, 0.9510565162951535312, 1.000000000000000000, 0.9510565162951535312, 1.000000000000000000, 0.9510565162951535312, 1.000000000000000000, 0.9510565162951535312, 1.000000000000000000, 0.9510565162951535312, 1.000000000000000000, 0.9510565162951535312, 1.000000000000000000, 0.9510565162951535312, 1.000000000000000000, 0.9510565162951535312, 1.000000000000000000, 0.9510565162951535312, 1.000000000000000000, 0.9510565162951535312, 1.000000000000000000, 0.9510565162951535312, 1.000000000000000000, 0.9510565162951535312, 1.000000000000000000, 0.9510565162951535312, 1.000000000000000000, 0.9510565162951535312, 1.000000000000000000, 0.9510565162951535312, 1.000000000000000000, 0.9510565162951535312, 1.000000000000000000, 0.9510565162951535312, 1.000000000000000000, 0.9510565162951535312, 1.000000000000000000, 0.9510565162951535312, 1.000000000000000000, 0.9510565162951535312, 1.000000000000000000, 0.9510565162951535312, 1.000000000000000000, 0.9510565162951535312, 1.000000000000000000, 0.9510565162951535312, 1.000000000000000000, 0.9510565162951535312, 1.000000000000000000, 0.9510565162951535312, 1.000000000000000000, 0.9510565162951535312, 1.000000000000000000, 0.9510565162951535312, 1.000000000000000000, 0.9510565162951535312, 1.000000000000000000, 0.9510565162951535312, 1.000000000000000000, 0.9510565162951535312, 1.000000000000000000, 0.9510565162951535312, 1.000000000000000000, 0.9510565162951535312, 1.000000000000000000, 0.9510565162951535312, 1.000000000000000000, 0.9510565162951535312, 1.000000000000000000, 0.9510565162951535312, 1.000000000000000000, 0.9510565162951535312, 1.000000000000000000, 0.9510565162951535312, 1.000000000000000000, 0.9510565162951535312, 1.000000000000000000, 0.9510565162951535312, 1.000000000000000000, 0.9510565162951535312, 1.000000000000000000, 0.9510565162951535312, 1.000000000000000000, 0.9510565162951535312, 1.000000000000000000, 0.9510565162951535312, 1.000000000000000000, 0.9510565162951535312, 1.000000000000000000, 0.9510565162951535312, 1.000000000000000000, 0.9510565162951535312, 1.000000000000000000, 0.9510565162951535312, 1.000000000000000000, 0.9510565162951535312, 1.000000000000000000, 0.9510565162951535312, 1.000000000000000000, 0.9510565162951535312, 1.000000000000000000, 0.9510565162951535312, 1.000000000000000000, 0.9510565162951535312, 1.000000000000000000, 0.9510565162951535312, 1.000000000000000000, 0.9510565162951535312, 1.000000000000000000, 0.9510565162951535312, 1.000000000000000000, 0.9510565162951535312, 1.000000000000000000, 0.9510565162951535312, 1.000000000000000000, 0.9510565162951535312, 1.000000000000000000, 0.9510565162951535312, 1.000000000000000000, 0.9510565162951535312, 1.000000000000000000, 0.9510565162951535312, 1.000000000000000000, 0.9510565162951535312, 1.000000000000000000, 0.9510565162951535312, 1.000000000000000000, 0.9510565162951535312, 1.000000000000000000, 0.9510565162951535312, 1.000000000000000000, 0.9510565162951535312, 1.000000000000000000, 0.9510565162951535312, 1.000000000000000000, 0.9510565162951535312, 1.000000000000000000, 0.9510565162951535312, 1.000000000000000000, 0.9510565162951535312, 1.000000000000000000, 0.9510565162951535312, 1.000000000000000000, 0.9510565162951535312, 1.000000000000000000, 0.9510565162951535312, 1.000000000000000000, 0.9510565162951535312, 1.000000000000000000, 0.9510565162951535312, 1.000000000000000000, 0.9510565162951535312, 1.000000000000000000, 0.9510565162951535312, 1.000000000000000000, 0.9510565162951535312, 1.000000000000000000, 0.9510565162951535312, 1.000000000000000000, 0.9510565162951535312, 1.000000000000000000, 0.9510565162951535312, 1.000000000000000000, 0.9510565162951535312, 1.000000000000000000),
 ( 0.3333333333333333703, 0.3170188387650512141, 0.3333333333333333703, 0.3170188387650512141, 0.3333333333333333703, 0.3170188387650512141, 0.3333333333333333703, 0.3170188387650512141, 0.3333333333333333703, 0.3170188387650512141, 0.3333333333333333703, 0.3170188387650512141, 0.3333333333333333703, 0.3170188387650512141, 0.3333333333333333703, 0.3170188387650512141, 0.3333333333333333703, 0.3170188387650512141, 0.3333333333333333703, 0.3170188387650512141, 0.3333333333333333703, 0.3170188387650512141, 0.3333333333333333703, 0.3170188387650512141, 0.3333333333333333703, 0.3170188387650512141, 0.3333333333333333703, 0.3170188387650512141, 0.3333333333333333703, 0.3170188387650512141, 0.3333333333333333703, 0.3170188387650512141, 0.3333333333333333703, 0.3170188387650512141, 0.3333333333333333703, 0.3170188387650512141, 0.3333333333333333703, 0.3170188387650512141, 0.3333333333333333703, 0.3170188387650512141, 0.3333333333333333703, 0.3170188387650512141, 0.3333333333333333703, 0.3170188387650512141, 0.3333333333333333703, 0.3170188387650512141, 0.3333333333333333703, 0.3170188387650512141, 0.3333333333333333703, 0.3170188387650512141, 0.3333333333333333703, 0.3170188387650512141, 0.3333333333333333703, 0.3170188387650512141, 0.3333333333333333703, 0.3170188387650512141, 0.3333333333333333703, 0.3170188387650512141, 0.3333333333333333703, 0.3170188387650512141, 0.3333333333333333703, 0.3170188387650512141, 0.3333333333333333703, 0.3170188387650512141, 0.3333333333333333703, 0.3170188387650512141, 0.3333333333333333703, 0.3170188387650512141, 0.3333333333333333703, 0.3170188387650512141, 0.3333333333333333703, 0.3170188387650512141, 0.3333333333333333703, 0.3170188387650512141, 0.3333333333333333703, 0.3170188387650512141, 0.3333333333333333703, 0.3170188387650512141, 0.3333333333333333703, 0.3170188387650512141, 0.3333333333333333703, 0.3170188387650512141, 0.3333333333333333703, 0.3170188387650512141, 0.3333333333333333703, 0.3170188387650512141, 0.3333333333333333703, 0.3170188387650512141, 0.3333333333333333703, 0.3170188387650512141, 0.3333333333333333703, 0.3170188387650512141, 0.3333333333333333703, 0.3170188387650512141, 0.3333333333333333703, 0.3170188387650512141, 0.3333333333333333703, 0.3170188387650512141, 0.3333333333333333703, 0.3170188387650512141, 0.3333333333333333703, 0.3170188387650512141, 0.3333333333333333703, 0.3170188387650512141, 0.3333333333333333703, 0.3170188387650512141, 0.3333333333333333703, 0.3170188387650512141, 0.3333333333333333703, 0.3170188387650512141, 0.3333333333333333703, 0.3170188387650512141, 0.3333333333333333703, 0.3170188387650512141, 0.3333333333333333703, 0.3170188387650512141, 0.3333333333333333703, 0.3170188387650512141, 0.3333333333333333703, 0.3170188387650512141, 0.3333333333333333703, 0.3170188387650512141, 0.3333333333333333703, 0.3170188387650512141, 0.3333333333333333703, 0.3170188387650512141, 0.3333333333333333703, 0.3170188387650512141, 0.3333333333333333703, 0.3170188387650512141, 0.3333333333333333703, 0.3170188387650512141, 0.3333333333333333703, 0.3170188387650512141, 0.3333333333333333703, 0.3170188387650512141, 0.3333333333333333703, 0.3170188387650512141, 0.3333333333333333703, 0.3170188387650512141, 0.3333333333333333703, 0.3170188387650512141, 0.3333333333333333703, 0.3170188387650512141, 0.3333333333333333703, 0.3170188387650512141, 0.3333333333333333703, 0.3170188387650512141, 0.3333333333333333703, 0.3170188387650512141, 0.3333333333333333703, 0.3170188387650512141, 0.3333333333333333703, 0.3170188387650512141, 0.3333333333333333703, 0.3170188387650512141, 0.3333333333333333703, 0.3170188387650512141, 0.3333333333333333703, 0.3170188387650512141, 0.3333333333333333703, 0.3170188387650512141, 0.3333333333333333703, 0.3170188387650512141, 0.3333333333333333703, 0.3170188387650512141, 0.3333333333333333703, 0.3170188387650512141, 0.3333333333333333703, 0.3170188387650512141, 0.3333333333333333703, 0.3170188387650512141, 0.3333333333333333703, 0.3170188387650512141, 0.3333333333333333703, 0.3170188387650512141, 0.3333333333333333703, 0.3170188387650512141, 0.3333333333333333703, 0.3170188387650512141, 0.3333333333333333703, 0.3170188387650512141, 0.3333333333333333703, 0.3170188387650512141, 0.3333333333333333703, 0.3170188387650512141, 0.3333333333333333703, 0.3170188387650512141, 0.3333333333333333703, 0.3170188387650512141, 0.3333333333333333703, 0.3170188387650512141, 0.3333333333333333703, 0.3170188387650512141, 0.3333333333333333703, 0.3170188387650512141, 0.3333333333333333703, 0.3170188387650512141, 0.3333333333333333703, 0.3170188387650512141, 0.3333333333333333703, 0.3170188387650512141, 0.3333333333333333703, 0.3170188387650512141, 0.3333333333333333703, 0.3170188387650512141, 0.3333333333333333703, 0.3170188387650512141, 0.3333333333333333703, 0.3170188387650512141, 0.3333333333333333703, 0.3170188387650512141, 0.3333333333333333703, 0.3170188387650512141, 0.3333333333333333703, 0.3170188387650512141, 0.3333333333333333703, 0.3170188387650512141, 0.3333333333333333703, 0.3170188387650512141, 0.3333333333333333703, 0.3170188387650512141, 0.3333333333333333703, 0.3170188387650512141, 0.3333333333333333703, 0.3170188387650512141, 0.3333333333333333703, 0.3170188387650512141, 0.3333333333333333703, 0.3170188387650512141, 0.3333333333333333703, 0.3170188387650512141, 0.3333333333333333703, 0.3170188387650512141, 0.3333333333333333703, 0.3170188387650512141, 0.3333333333333333703, 0.3170188387650512141, 0.3333333333333333703, 0.3170188387650512141, 0.3333333333333333703, 0.3170188387650512141, 0.3333333333333333703, 0.3170188387650512141, 0.3333333333333333703, 0.3170188387650512141, 0.3333333333333333703, 0.3170188387650512141, 0.3333333333333333703, 0.3170188387650512141, 0.3333333333333333703, 0.3170188387650512141, 0.3333333333333333703, 0.3170188387650512141, 0.3333333333333333703, 0.3170188387650512141, 0.3333333333333333703, 0.3170188387650512141, 0.3333333333333333703, 0.3170188387650512141, 0.3333333333333333703),
 ( 0.3333333333333333703, 0.3170188387650512141, 0.3333333333333333703, 0.3170188387650512141, 0.3333333333333333703, 0.3170188387650512141, 0.3333333333333333703, 0.3170188387650512141, 0.3333333333333333703, 0.3170188387650512141, 0.3333333333333333703, 0.3170188387650512141, 0.3333333333333333703, 0.3170188387650512141, 0.3333333333333333703, 0.3170188387650512141, 0.3333333333333333703, 0.3170188387650512141, 0.3333333333333333703, 0.3170188387650512141, 0.3333333333333333703, 0.3170188387650512141, 0.3333333333333333703, 0.3170188387650512141, 0.3333333333333333703, 0.3170188387650512141, 0.3333333333333333703, 0.3170188387650512141, 0.3333333333333333703, 0.3170188387650512141, 0.3333333333333333703, 0.3170188387650512141, 0.3333333333333333703, 0.3170188387650512141, 0.3333333333333333703, 0.3170188387650512141, 0.3333333333333333703, 0.3170188387650512141, 0.3333333333333333703, 0.3170188387650512141, 0.3333333333333333703, 0.3170188387650512141, 0.3333333333333333703, 0.3170188387650512141, 0.3333333333333333703, 0.3170188387650512141, 0.3333333333333333703, 0.3170188387650512141, 0.3333333333333333703, 0.3170188387650512141, 0.3333333333333333703, 0.3170188387650512141, 0.3333333333333333703, 0.3170188387650512141, 0.3333333333333333703, 0.3170188387650512141, 0.3333333333333333703, 0.3170188387650512141, 0.3333333333333333703, 0.3170188387650512141, 0.3333333333333333703, 0.3170188387650512141, 0.3333333333333333703, 0.3170188387650512141, 0.3333333333333333703, 0.3170188387650512141, 0.3333333333333333703, 0.3170188387650512141, 0.3333333333333333703, 0.3170188387650512141, 0.3333333333333333703, 0.3170188387650512141, 0.3333333333333333703, 0.3170188387650512141, 0.3333333333333333703, 0.3170188387650512141, 0.3333333333333333703, 0.3170188387650512141, 0.3333333333333333703, 0.3170188387650512141, 0.3333333333333333703, 0.3170188387650512141, 0.3333333333333333703, 0.3170188387650512141, 0.3333333333333333703, 0.3170188387650512141, 0.3333333333333333703, 0.3170188387650512141, 0.3333333333333333703, 0.3170188387650512141, 0.3333333333333333703, 0.3170188387650512141, 0.3333333333333333703, 0.3170188387650512141, 0.3333333333333333703, 0.3170188387650512141, 0.3333333333333333703, 0.3170188387650512141, 0.3333333333333333703, 0.3170188387650512141, 0.3333333333333333703, 0.3170188387650512141, 0.3333333333333333703, 0.3170188387650512141, 0.3333333333333333703, 0.3170188387650512141, 0.3333333333333333703, 0.3170188387650512141, 0.3333333333333333703, 0.3170188387650512141, 0.3333333333333333703, 0.3170188387650512141, 0.3333333333333333703, 0.3170188387650512141, 0.3333333333333333703, 0.3170188387650512141, 0.3333333333333333703, 0.3170188387650512141, 0.3333333333333333703, 0.3170188387650512141, 0.3333333333333333703, 0.3170188387650512141, 0.3333333333333333703, 0.3170188387650512141, 0.3333333333333333703, 0.3170188387650512141, 0.3333333333333333703, 0.3170188387650512141, 0.3333333333333333703, 0.3170188387650512141, 0.3333333333333333703, 0.3170188387650512141, 0.3333333333333333703, 0.3170188387650512141, 0.3333333333333333703, 0.3170188387650512141, 0.3333333333333333703, 0.3170188387650512141, 0.3333333333333333703, 0.3170188387650512141, 0.3333333333333333703, 0.3170188387650512141, 0.3333333333333333703, 0.3170188387650512141, 0.3333333333333333703, 0.3170188387650512141, 0.3333333333333333703, 0.3170188387650512141, 0.3333333333333333703, 0.3170188387650512141, 0.3333333333333333703, 0.3170188387650512141, 0.3333333333333333703, 0.3170188387650512141, 0.3333333333333333703, 0.3170188387650512141, 0.3333333333333333703, 0.3170188387650512141, 0.3333333333333333703, 0.3170188387650512141, 0.3333333333333333703, 0.3170188387650512141, 0.3333333333333333703, 0.3170188387650512141, 0.3333333333333333703, 0.3170188387650512141, 0.3333333333333333703, 0.3170188387650512141, 0.3333333333333333703, 0.3170188387650512141, 0.3333333333333333703, 0.3170188387650512141, 0.3333333333333333703, 0.3170188387650512141, 0.3333333333333333703, 0.3170188387650512141, 0.3333333333333333703, 0.3170188387650512141, 0.3333333333333333703, 0.3170188387650512141, 0.3333333333333333703, 0.3170188387650512141, 0.3333333333333333703, 0.3170188387650512141, 0.3333333333333333703, 0.3170188387650512141, 0.3333333333333333703, 0.3170188387650512141, 0.3333333333333333703, 0.3170188387650512141, 0.3333333333333333703, 0.3170188387650512141, 0.3333333333333333703, 0.3170188387650512141, 0.3333333333333333703, 0.3170188387650512141, 0.3333333333333333703, 0.3170188387650512141, 0.3333333333333333703, 0.3170188387650512141, 0.3333333333333333703, 0.3170188387650512141, 0.3333333333333333703, 0.3170188387650512141, 0.3333333333333333703, 0.3170188387650512141, 0.3333333333333333703, 0.3170188387650512141, 0.3333333333333333703, 0.3170188387650512141, 0.3333333333333333703, 0.3170188387650512141, 0.3333333333333333703, 0.3170188387650512141, 0.3333333333333333703, 0.3170188387650512141, 0.3333333333333333703, 0.3170188387650512141, 0.3333333333333333703, 0.3170188387650512141, 0.3333333333333333703, 0.3170188387650512141, 0.3333333333333333703, 0.3170188387650512141, 0.3333333333333333703, 0.3170188387650512141, 0.3333333333333333703, 0.3170188387650512141, 0.3333333333333333703, 0.3170188387650512141, 0.3333333333333333703, 0.3170188387650512141, 0.3333333333333333703, 0.3170188387650512141, 0.3333333333333333703, 0.3170188387650512141, 0.3333333333333333703, 0.3170188387650512141, 0.3333333333333333703, 0.3170188387650512141, 0.3333333333333333703, 0.3170188387650512141, 0.3333333333333333703, 0.3170188387650512141, 0.3333333333333333703, 0.3170188387650512141, 0.3333333333333333703, 0.3170188387650512141, 0.3333333333333333703, 0.3170188387650512141, 0.3333333333333333703, 0.3170188387650512141, 0.3333333333333333703, 0.3170188387650512141, 0.3333333333333333703, 0.3170188387650512141, 0.3333333333333333703, 0.3170188387650512141, 0.3333333333333333703, 0.3170188387650512141, 0.3333333333333333703),
 ( 1.000000000000000000, 0.9510565162951535312, 1.000000000000000000, 0.9510565162951535312, 1.000000000000000000, 0.9510565162951535312, 1.000000000000000000, 0.9510565162951535312, 1.000000000000000000, 0.9510565162951535312, 1.000000000000000000, 0.9510565162951535312, 1.000000000000000000, 0.9510565162951535312, 1.000000000000000000, 0.9510565162951535312, 1.000000000000000000, 0.9510565162951535312, 1.000000000000000000, 0.9510565162951535312, 1.000000000000000000, 0.9510565162951535312, 1.000000000000000000, 0.9510565162951535312, 1.000000000000000000, 0.9510565162951535312, 1.000000000000000000, 0.9510565162951535312, 1.000000000000000000, 0.9510565162951535312, 1.000000000000000000, 0.9510565162951535312, 1.000000000000000000, 0.9510565162951535312, 1.000000000000000000, 0.9510565162951535312, 1.000000000000000000, 0.9510565162951535312, 1.000000000000000000, 0.9510565162951535312, 1.000000000000000000, 0.9510565162951535312, 1.000000000000000000, 0.9510565162951535312, 1.000000000000000000, 0.9510565162951535312, 1.000000000000000000, 0.9510565162951535312, 1.000000000000000000, 0.9510565162951535312, 1.000000000000000000, 0.9510565162951535312, 1.000000000000000000, 0.9510565162951535312, 1.000000000000000000, 0.9510565162951535312, 1.000000000000000000, 0.9510565162951535312, 1.000000000000000000, 0.9510565162951535312, 1.000000000000000000, 0.9510565162951535312, 1.000000000000000000, 0.9510565162951535312, 1.000000000000000000, 0.9510565162951535312, 1.000000000000000000, 0.9510565162951535312, 1.000000000000000000, 0.9510565162951535312, 1.000000000000000000, 0.9510565162951535312, 1.000000000000000000, 0.9510565162951535312, 1.000000000000000000, 0.9510565162951535312, 1.000000000000000000, 0.9510565162951535312, 1.000000000000000000, 0.9510565162951535312, 1.000000000000000000, 0.9510565162951535312, 1.000000000000000000, 0.9510565162951535312, 1.000000000000000000, 0.9510565162951535312, 1.000000000000000000, 0.9510565162951535312, 1.000000000000000000, 0.9510565162951535312, 1.000000000000000000, 0.9510565162951535312, 1.000000000000000000, 0.9510565162951535312, 1.000000000000000000, 0.9510565162951535312, 1.000000000000000000, 0.9510565162951535312, 1.000000000000000000, 0.9510565162951535312, 1.000000000000000000, 0.9510565162951535312, 1.000000000000000000, 0.9510565162951535312, 1.000000000000000000, 0.9510565162951535312, 1.000000000000000000, 0.9510565162951535312, 1.000000000000000000, 0.9510565162951535312, 1.000000000000000000, 0.9510565162951535312, 1.000000000000000000, 0.9510565162951535312, 1.000000000000000000, 0.9510565162951535312, 1.000000000000000000, 0.9510565162951535312, 1.000000000000000000, 0.9510565162951535312, 1.000000000000000000, 0.9510565162951535312, 1.000000000000000000, 0.9510565162951535312, 1.000000000000000000, 0.9510565162951535312, 1.000000000000000000, 0.9510565162951535312, 1.000000000000000000, 0.9510565162951535312, 1.000000000000000000, 0.9510565162951535312, 1.000000000000000000, 0.9510565162951535312, 1.000000000000000000, 0.9510565162951535312, 1.000000000000000000, 0.9510565162951535312, 1.000000000000000000, 0.9510565162951535312, 1.000000000000000000, 0.9510565162951535312, 1.000000000000000000, 0.9510565162951535312, 1.000000000000000000, 0.9510565162951535312, 1.000000000000000000, 0.9510565162951535312, 1.000000000000000000, 0.9510565162951535312, 1.000000000000000000, 0.9510565162951535312, 1.000000000000000000, 0.9510565162951535312, 1.000000000000000000, 0.9510565162951535312, 1.000000000000000000, 0.9510565162951535312, 1.000000000000000000, 0.9510565162951535312, 1.000000000000000000, 0.9510565162951535312, 1.000000000000000000, 0.9510565162951535312, 1.000000000000000000, 0.9510565162951535312, 1.000000000000000000, 0.9510565162951535312, 1.000000000000000000, 0.9510565162951535312, 1.000000000000000000, 0.9510565162951535312, 1.000000000000000000, 0.9510565162951535312, 1.000000000000000000, 0.9510565162951535312, 1.000000000000000000, 0.9510565162951535312, 1.000000000000000000, 0.9510565162951535312, 1.000000000000000000, 0.9510565162951535312, 1.000000000000000000, 0.9510565162951535312, 1.000000000000000000, 0.9510565162951535312, 1.000000000000000000, 0.9510565162951535312, 1.000000000000000000, 0.9510565162951535312, 1.000000000000000000, 0.9510565162951535312, 1.000000000000000000, 0.9510565162951535312, 1.000000000000000000, 0.9510565162951535312, 1.000000000000000000, 0.9510565162951535312, 1.000000000000000000, 0.9510565162951535312, 1.000000000000000000, 0.9510565162951535312, 1.000000000000000000, 0.9510565162951535312, 1.000000000000000000, 0.9510565162951535312, 1.000000000000000000, 0.9510565162951535312, 1.000000000000000000, 0.9510565162951535312, 1.000000000000000000, 0.9510565162951535312, 1.000000000000000000, 0.9510565162951535312, 1.000000000000000000, 0.9510565162951535312, 1.000000000000000000, 0.9510565162951535312, 1.000000000000000000, 0.9510565162951535312, 1.000000000000000000, 0.9510565162951535312, 1.000000000000000000, 0.9510565162951535312, 1.000000000000000000, 0.9510565162951535312, 1.000000000000000000, 0.9510565162951535312, 1.000000000000000000, 0.9510565162951535312, 1.000000000000000000, 0.9510565162951535312, 1.000000000000000000, 0.9510565162951535312, 1.000000000000000000, 0.9510565162951535312, 1.000000000000000000, 0.9510565162951535312, 1.000000000000000000, 0.9510565162951535312, 1.000000000000000000, 0.9510565162951535312, 1.000000000000000000, 0.9510565162951535312, 1.000000000000000000, 0.9510565162951535312, 1.000000000000000000, 0.9510565162951535312, 1.000000000000000000, 0.9510565162951535312, 1.000000000000000000, 0.9510565162951535312, 1.000000000000000000, 0.9510565162951535312, 1.000000000000000000, 0.9510565162951535312, 1.000000000000000000, 0.9510565162951535312, 1.000000000000000000, 0.9510565162951535312, 1.000000000000000000) ) ) 
 REPRESENTATION_ITEM ( '' )  SURFACE ( )  );
#5961 = ITEM_DEFINED_TRANSFORMATION ( 'NONE', 'NONE', #1608,  #2840 ) ;
#5962 = CARTESIAN_POINT ( 'NONE',  ( -5.257311121191324155, -74.74547149457075079, -0.09995255151718371311 ) ) ;
#5963 = ADVANCED_FACE ( 'NONE', ( #7964 ), #957, .T. ) ;
#5964 = LINE ( 'NONE', #6635, #1073 ) ;
#5965 = CARTESIAN_POINT ( 'NONE',  ( 2.862020680886601998, -96.79547149457073374, 4.100960146803977580 ) ) ;
#5966 = CARTESIAN_POINT ( 'NONE',  ( 6.013306294175168709, -67.95452850542925205, 4.245374608440616093 ) ) ;
#5967 = CARTESIAN_POINT ( 'NONE',  ( 50.00000000000000000, -7.999999999999996447, 12.49999999999999822 ) ) ;
#5968 = AXIS2_PLACEMENT_3D ( 'NONE', #605, #6426, #6511 ) ;
#5969 = VECTOR ( 'NONE', #764, 1000.000000000000000 ) ;
#5970 = DIRECTION ( 'NONE',  ( -0.5000000000000011102, 0.8660254037844380415, 0.000000000000000000 ) ) ;
#5971 = CARTESIAN_POINT ( 'NONE',  ( 4.312004677471078296, -85.95452850542925205, 3.009306630940844496 ) ) ;
#5972 = CARTESIAN_POINT ( 'NONE',  ( -2.179377348189463159, -64.35452850542924352, 7.030887037049988741 ) ) ;
#5973 = CARTESIAN_POINT ( 'NONE',  ( 2.493201789345310004, -78.94547149457073942, 1.934965279058241006 ) ) ;
#5974 = VECTOR ( 'NONE', #2444, 1000.000000000000000 ) ;
#5975 = STYLED_ITEM ( 'NONE', ( #1149 ), #7136 ) ;
#5976 = ORIENTED_EDGE ( 'NONE', *, *, #7898, .F. ) ;
#5977 = LINE ( 'NONE', #2189, #2880 ) ;
#5978 = CARTESIAN_POINT ( 'NONE',  ( -2.862020680886492308, -94.20452850542926626, 4.100960146804039752 ) ) ;
#5979 = CARTESIAN_POINT ( 'NONE',  ( 5.257311121191342806, -89.25452850542924921, -0.09995255151729465215 ) ) ;
#5980 = VERTEX_POINT ( 'NONE', #5932 ) ;
#5981 = CARTESIAN_POINT ( 'NONE',  ( 4.784657899331209663, -74.10452850542925773, 1.454677039711774533 ) ) ;
#5982 = CARTESIAN_POINT ( 'NONE',  ( -0.8796985632579406023, -95.14547149457074227, -3.030887037049952326 ) ) ;
#5983 = AXIS2_PLACEMENT_3D ( 'NONE', #5825, #5154, #5071 ) ;
#5984 = CARTESIAN_POINT ( 'NONE',  ( 2.862020680886514956, -83.70452850542925205, -4.100960146804039752 ) ) ;
#5985 = CARTESIAN_POINT ( 'NONE',  ( 4.191402346623199549, -94.80452850542926058, 5.607243785695311900 ) ) ;
#5986 = CARTESIAN_POINT ( 'NONE',  ( -0.09506052544082083111, -63.00452850542925631, -2.999999999999997780 ) ) ;
#5987 = ORIENTED_EDGE ( 'NONE', *, *, #4522, .T. ) ;
#5988 = DIRECTION ( 'NONE',  ( 0.000000000000000000, -1.000000000000000000, -2.168404344971009854E-16 ) ) ;
#5989 = CARTESIAN_POINT ( 'NONE',  ( 46.49999999999999289, -14.99999999999999467, 4.500000000000000888 ) ) ;
#5990 = CARTESIAN_POINT ( 'NONE',  ( -0.8796985632578785408, -82.35452850542927195, 3.030887037049973198 ) ) ;
#5991 = CARTESIAN_POINT ( 'NONE',  ( 6.686770931921525829, -92.10452850542925773, 2.072711028461649008 ) ) ;
#5992 = CARTESIAN_POINT ( 'NONE',  ( -7.360235569667856304, -92.74547149457073658, -0.09995255151716124498 ) ) ;
#5993 = LINE ( 'NONE', #976, #3603 ) ;
#5994 = LINE ( 'NONE', #4055, #5813 ) ;
#5995 = EDGE_CURVE ( 'NONE', #4617, #6264, #2108, .T. ) ;
#5996 = CARTESIAN_POINT ( 'NONE',  ( -0.09506052544075706268, -72.49547149457075079, 2.999999999999997780 ) ) ;
#5997 = ORIENTED_EDGE ( 'NONE', *, *, #7555, .T. ) ;
#5998 = CARTESIAN_POINT ( 'NONE',  ( -2.862020680886495416, -67.20452850542925205, 4.100960146804039752 ) ) ;
#5999 = CARTESIAN_POINT ( 'NONE',  ( 6.686770931921477867, -79.39547149457074227, -2.072711028461788896 ) ) ;
#6000 = ADVANCED_FACE ( 'NONE', ( #3413 ), #7282, .F. ) ;
#6001 = ORIENTED_EDGE ( 'NONE', *, *, #6746, .F. ) ;
#6002 = CARTESIAN_POINT ( 'NONE',  ( -1.529537955723671683, -64.35452850542924352, 5.030887037049979860 ) ) ;
#6003 = LINE ( 'NONE', #5367, #4490 ) ;
#6004 = CONTEXT_DEPENDENT_SHAPE_REPRESENTATION ( #4268, #8146 ) ;
#6005 = CARTESIAN_POINT ( 'NONE',  ( 4.784657899331176800, -73.39547149457074227, -1.454677039711874009 ) ) ;
#6006 = LINE ( 'NONE', #2266, #267 ) ;
#6007 = CARTESIAN_POINT ( 'NONE',  ( -1.069819614139476460, -60.34547149457074511, 2.969112962950044121 ) ) ;
#6008 = CARTESIAN_POINT ( 'NONE',  ( -6.628020296210623385, -63.90452850542925489, 2.253526892787613978 ) ) ;
#6009 = ORIENTED_EDGE ( 'NONE', *, *, #7387, .T. ) ;
#6010 = DIRECTION ( 'NONE',  ( -0.000000000000000000, -0.000000000000000000, -1.000000000000000000 ) ) ;
#6011 = CARTESIAN_POINT ( 'NONE',  ( 4.784657899331210551, -83.10452850542927195, 1.454677039711774533 ) ) ;
#6012 = CARTESIAN_POINT ( 'NONE',  ( 4.037591185471440802, -62.70452850542925916, -5.718994135553947977 ) ) ;
#6013 = CARTESIAN_POINT ( 'NONE',  ( 0.8796985632579624736, -81.64547149457074227, 3.030887037049952326 ) ) ;
#6014 = ORIENTED_EDGE ( 'NONE', *, *, #2957, .T. ) ;
#6015 = DIRECTION ( 'NONE',  ( -0.000000000000000000, -0.7071067811865507924, -0.7071067811865441310 ) ) ;
#6016 = PLANE ( 'NONE',  #7321 ) ;
#6017 = CARTESIAN_POINT ( 'NONE',  ( -5.257311121191324155, -78.75452850542924921, 0.09995255151729526277 ) ) ;
#6018 = ORIENTED_EDGE ( 'NONE', *, *, #4808, .F. ) ;
#6019 = CARTESIAN_POINT ( 'NONE',  ( -1.529537955723670795, -73.35452850542924352, 5.030887037049979860 ) ) ;
#6020 = CARTESIAN_POINT ( 'NONE',  ( -1.686450176301615977, -86.29547149457074795, -2.482926158054096000 ) ) ;
#6021 = CARTESIAN_POINT ( 'NONE',  ( -1.686450176301618864, -62.29547149457074084, -2.482926158054096000 ) ) ;
#6022 = CARTESIAN_POINT ( 'NONE',  ( 4.784657899331209663, -74.10452850542925773, 1.454677039711774533 ) ) ;
#6023 = CARTESIAN_POINT ( 'NONE',  ( -6.628020296210619833, -87.90452850542926910, 2.253526892787613978 ) ) ;
#6024 = CARTESIAN_POINT ( 'NONE',  ( -1.069819614139539521, -69.15452850542926910, -2.969112962950023249 ) ) ;
#6025 = EDGE_CURVE ( 'NONE', #26, #1714, #7044, .T. ) ;
#6026 = EDGE_LOOP ( 'NONE', ( #4578, #6504, #4152, #1638 ) ) ;
#6027 = CARTESIAN_POINT ( 'NONE',  ( 47.50000000000002132, -51.00000000000000711, -12.50000000000001954 ) ) ;
#6028 = CYLINDRICAL_SURFACE ( 'NONE', #5512, 1.499999999999999556 ) ;
#6029 = CARTESIAN_POINT ( 'NONE',  ( -1.069819614139537967, -78.15452850542924068, -2.969112962950023249 ) ) ;
#6030 = CARTESIAN_POINT ( 'NONE',  ( -2.369498399071205963, -87.15452850542926910, -6.969112962950009482 ) ) ;
#6031 = ADVANCED_FACE ( 'NONE', ( #6648 ), #7361, .T. ) ;
#6032 = CARTESIAN_POINT ( 'NONE',  ( -6.628020296210665130, -89.59547149457074511, -2.253526892787471869 ) ) ;
#6033 = LINE ( 'NONE', #6701, #6157 ) ;
#6034 = FACE_OUTER_BOUND ( 'NONE', #2496, .T. ) ;
#6035 = CARTESIAN_POINT ( 'NONE',  ( 2.823794231030058555, -67.09547149457073090, 1.017458915287723809 ) ) ;
#6036 = UNCERTAINTY_MEASURE_WITH_UNIT (LENGTH_MEASURE( 1.000000000000000082E-05 ), #772, 'distance_accuracy_value', 'NONE');
#6037 =( NAMED_UNIT ( * ) PLANE_ANGLE_UNIT ( ) SI_UNIT ( $, .RADIAN. ) );
#6038 = ORIENTED_EDGE ( 'NONE', *, *, #3633, .F. ) ;
#6039 = CARTESIAN_POINT ( 'NONE',  ( -5.257311121191324155, -66.75452850542923500, 0.09995255151729526277 ) ) ;
#6040 = CARTESIAN_POINT ( 'NONE',  ( -4.191402346623058328, -78.19547149457073942, 5.607243785695398941 ) ) ;
#6041 = EDGE_LOOP ( 'NONE', ( #4643, #880 ) ) ;
#6042 = CARTESIAN_POINT ( 'NONE',  ( -5.257311121191325043, -71.74547149457075079, -0.09995255151718372699 ) ) ;
#6043 = CARTESIAN_POINT ( 'NONE',  ( 4.784657899331208775, -65.10452850542924352, 1.454677039711774533 ) ) ;
#6044 = FACE_OUTER_BOUND ( 'NONE', #6928, .T. ) ;
#6045 = AXIS2_PLACEMENT_3D ( 'NONE', #678, #4591, #4508 ) ;
#6046 = CIRCLE ( 'NONE', #7391, 4.000000000000000000 ) ;
#6047 =( GEOMETRIC_REPRESENTATION_CONTEXT ( 3 ) GLOBAL_UNCERTAINTY_ASSIGNED_CONTEXT ( ( #219 ) ) GLOBAL_UNIT_ASSIGNED_CONTEXT ( ( #2470, #5072, #5554 ) ) REPRESENTATION_CONTEXT ( 'NONE', 'WORKASPACE' ) );
#6048 = CARTESIAN_POINT ( 'NONE',  ( 1.529537955723794695, -66.64547149457071384, 5.030887037049945221 ) ) ;
#6049 = CARTESIAN_POINT ( 'NONE',  ( 40.00000000000000000, -9.999999999999992895, 4.499999999999999112 ) ) ;
#6050 = CARTESIAN_POINT ( 'NONE',  ( -4.312004677470990366, -96.04547149457074795, 3.009306630940933758 ) ) ;
#6051 = CARTESIAN_POINT ( 'NONE',  ( -2.179377348189463603, -61.35452850542925773, 7.030887037049988741 ) ) ;
#6052 = EDGE_LOOP ( 'NONE', ( #3241, #6363, #8136, #5957 ) ) ;
#6053 = DIRECTION ( 'NONE',  ( -0.000000000000000000, 2.775557561562891351E-16, -1.000000000000000000 ) ) ;
#6054 = CARTESIAN_POINT ( 'NONE',  ( 4.725907263620340970, -80.40452850542925489, -1.635492904037697981 ) ) ;
#6055 = AXIS2_PLACEMENT_3D ( 'NONE', #2077, #4632, #6492 ) ;
#6056 = ORIENTED_EDGE ( 'NONE', *, *, #3253, .T. ) ;
#6057 = FACE_OUTER_BOUND ( 'NONE', #7776, .T. ) ;
#6058 = CARTESIAN_POINT ( 'NONE',  ( 4.194503406049339134, -89.55452850542926058, -3.171033256558100089 ) ) ;
#6059 = CARTESIAN_POINT ( 'NONE',  ( 4.312004677471076519, -82.95452850542925205, 3.009306630940844496 ) ) ;
#6060 = EDGE_CURVE ( 'NONE', #6402, #26, #5977, .T. ) ;
#6061 = EDGE_LOOP ( 'NONE', ( #4338, #1219, #1622, #4225 ) ) ;
#6062 = CARTESIAN_POINT ( 'NONE',  ( -5.257311121191325043, -69.75452850542926342, 0.09995255151729529053 ) ) ;
#6063 = CARTESIAN_POINT ( 'NONE',  ( 2.882544866740879730, -94.39547149457074227, -0.8366430509619593447 ) ) ;
#6064 = CARTESIAN_POINT ( 'NONE',  ( -2.610703060766927930, -60.04547149457073374, 1.773238653441125745 ) ) ;
#6065 = CARTESIAN_POINT ( 'NONE',  ( -3.015831842038214639, -78.30452850542926058, -3.989209796945429432 ) ) ;
#6066 = CARTESIAN_POINT ( 'NONE',  ( 0.09506052544088250400, -85.50452850542926342, 6.999999999999997335 ) ) ;
#6067 = CARTESIAN_POINT ( 'NONE',  ( -0.09506052544075405120, -96.49547149457075079, 2.999999999999997780 ) ) ;
#6068 = ORIENTED_EDGE ( 'NONE', *, *, #1776, .T. ) ;
#6069 = LINE ( 'NONE', #3462, #649 ) ;
#6070 = VERTEX_POINT ( 'NONE', #2271 ) ;
#6071 = CARTESIAN_POINT ( 'NONE',  ( 50.00000000000000000, -9.999999999999994671, 0.000000000000000000 ) ) ;
#6072 = CARTESIAN_POINT ( 'NONE',  ( 1.069819614139557062, -76.65452850542925489, 2.969112962950023249 ) ) ;
#6073 = CARTESIAN_POINT ( 'NONE',  ( 0.09506052544088290646, -88.50452850542926342, 6.999999999999997335 ) ) ;
#6074 = CARTESIAN_POINT ( 'NONE',  ( 2.179377348189630137, -81.64547149457074227, 7.030887037049939003 ) ) ;
#6075 = DIRECTION ( 'NONE',  ( 1.000000000000000000, 1.261617073437677752E-16, 0.000000000000000000 ) ) ;
#6076 = CARTESIAN_POINT ( 'NONE',  ( -2.862020680886578461, -95.29547149457074795, -4.100960146803977580 ) ) ;
#6077 = CARTESIAN_POINT ( 'NONE',  ( 1.686450176301586668, -86.70452850542925205, -2.482926158054133303 ) ) ;
#6078 = DIRECTION ( 'NONE',  ( -1.000000000000000000, 0.000000000000000000, 0.000000000000000000 ) ) ;
#6079 = VERTEX_POINT ( 'NONE', #1469 ) ;
#6080 = CARTESIAN_POINT ( 'NONE',  ( 50.00000000000000000, -9.999999999999992895, 4.499999999999999112 ) ) ;
#6081 = CARTESIAN_POINT ( 'NONE',  ( -4.725907263620323207, -63.90452850542925489, 1.635492904037698647 ) ) ;
#6082 = CARTESIAN_POINT ( 'NONE',  ( 6.686770931921479644, -82.39547149457074227, -2.072711028461788896 ) ) ;
#6083 = ORIENTED_EDGE ( 'NONE', *, *, #1752, .F. ) ;
#6084 = CARTESIAN_POINT ( 'NONE',  ( -4.312004677470993030, -78.04547149457076216, 3.009306630940933314 ) ) ;
#6085 = CARTESIAN_POINT ( 'NONE',  ( 4.784657899331176800, -67.39547149457074227, -1.454677039711874009 ) ) ;
#6086 = CARTESIAN_POINT ( 'NONE',  ( 3.015831842038232846, -67.80452850542926058, 3.989209796945429432 ) ) ;
#6087 = DIRECTION ( 'NONE',  ( 1.000000000000000000, -0.000000000000000000, -0.000000000000000000 ) ) ;
#6088 = EDGE_CURVE ( 'NONE', #6860, #3650, #5422, .T. ) ;
#6089 = CARTESIAN_POINT ( 'NONE',  ( 4.312004677471011682, -70.54547149457074795, -3.009306630940933314 ) ) ;
#6090 = CARTESIAN_POINT ( 'NONE',  ( -2.179377348189463603, -58.35452850542927195, 7.030887037049988741 ) ) ;
#6091 = EDGE_LOOP ( 'NONE', ( #6160, #3482, #2323, #2213 ) ) ;
#6092 = ADVANCED_FACE ( 'NONE', ( #6057 ), #6094, .T. ) ;
#6093 = ORIENTED_EDGE ( 'NONE', *, *, #1520, .F. ) ;
#6094 = PLANE ( 'NONE',  #3951 ) ;
#6095 = CARTESIAN_POINT ( 'NONE',  ( -1.719659006605370744, -90.15452850542922647, -4.969112962950016588 ) ) ;
#6096 = CARTESIAN_POINT ( 'NONE',  ( -1.529537955723670350, -76.35452850542925773, 5.030887037049979860 ) ) ;
#6097 = VERTEX_POINT ( 'NONE', #4076 ) ;
#6098 = CARTESIAN_POINT ( 'NONE',  ( 3.015831842038232846, -67.80452850542926058, 3.989209796945429432 ) ) ;
#6099 = CARTESIAN_POINT ( 'NONE',  ( -2.882544866740857081, -80.89547149457074227, 0.8366430509619596778 ) ) ;
#6100 = CARTESIAN_POINT ( 'NONE',  ( -1.069819614139476460, -60.34547149457074511, 2.969112962950044121 ) ) ;
#6101 = CARTESIAN_POINT ( 'NONE',  ( 0.09506052544085971667, -73.50452850542924921, 4.999999999999997335 ) ) ;
#6102 = CARTESIAN_POINT ( 'NONE',  ( 6.013306294175171374, -85.95452850542925205, 4.245374608440616093 ) ) ;
#6103 =( GEOMETRIC_REPRESENTATION_CONTEXT ( 3 ) GLOBAL_UNCERTAINTY_ASSIGNED_CONTEXT ( ( #7487 ) ) GLOBAL_UNIT_ASSIGNED_CONTEXT ( ( #4899, #6037, #1657 ) ) REPRESENTATION_CONTEXT ( 'NONE', 'WORKASPACE' ) );
#6104 = CIRCLE ( 'NONE', #5559, 4.000000000000000000 ) ;
#6105 = CARTESIAN_POINT ( 'NONE',  ( 0.8796985632579640280, -93.64547149457074227, 3.030887037049952326 ) ) ;
#6106 = ORIENTED_EDGE ( 'NONE', *, *, #3219, .F. ) ;
#6107 = CARTESIAN_POINT ( 'NONE',  ( -47.50000000000000711, -46.99999999999998579, 12.49999999999993960 ) ) ;
#6108 = VECTOR ( 'NONE', #990, 1000.000000000000114 ) ;
#6109 = CARTESIAN_POINT ( 'NONE',  ( 1.529537955723692999, -95.85452850542924352, -5.030887037049978971 ) ) ;
#6110 = CARTESIAN_POINT ( 'NONE',  ( -1.686450176301566017, -73.20452850542925205, 2.482926158054133303 ) ) ;
#6111 = CARTESIAN_POINT ( 'NONE',  ( -2.369498399071205963, -84.15452850542925489, -6.969112962950009482 ) ) ;
#6112 = CARTESIAN_POINT ( 'NONE',  ( -6.686770931921458327, -80.89547149457074227, 2.072711028461789784 ) ) ;
#6113 = PLANE ( 'NONE',  #637 ) ;
#6114 = CARTESIAN_POINT ( 'NONE',  ( -0.09506052544073315125, -93.49547149457073658, 4.999999999999997335 ) ) ;
#6115 = CARTESIAN_POINT ( 'NONE',  ( 2.610703060766985217, -88.95452850542925205, 1.773238653441072232 ) ) ;
#6116 = VECTOR ( 'NONE', #6053, 1000.000000000000000 ) ;
#6117 = UNCERTAINTY_MEASURE_WITH_UNIT (LENGTH_MEASURE( 1.000000000000000082E-05 ), #1409, 'distance_accuracy_value', 'NONE');
#6118 = VERTEX_POINT ( 'NONE', #2232 ) ;
#6119 = VECTOR ( 'NONE', #5407, 1000.000000000000000 ) ;
#6120 = DIRECTION ( 'NONE',  ( 0.9662349396012460678, 0.2576626505603332173, 0.000000000000000000 ) ) ;
#6121 = CARTESIAN_POINT ( 'NONE',  ( -4.312004677471060532, -63.45452850542926626, -3.009306630940844052 ) ) ;
#6122 = CARTESIAN_POINT ( 'NONE',  ( -5.895805022753476621, -83.44547149457073942, -4.407101234057782868 ) ) ;
#6123 = ORIENTED_EDGE ( 'NONE', *, *, #8335, .T. ) ;
#6124 = CARTESIAN_POINT ( 'NONE',  ( -0.09506052544073503863, -78.49547149457073658, 4.999999999999997335 ) ) ;
#6125 = CARTESIAN_POINT ( 'NONE',  ( 4.725907263620372056, -73.09547149457074511, 1.635492904037598283 ) ) ;
#6126 = CARTESIAN_POINT ( 'NONE',  ( 1.719659006605388507, -61.65452850542923358, 4.969112962950016588 ) ) ;
#6127 = CARTESIAN_POINT ( 'NONE',  ( 50.00000000000000000, -12.00000000000000711, 12.49999999999999822 ) ) ;
#6128 = ADVANCED_FACE ( 'NONE', ( #7410, #1551 ), #4115, .F. ) ;
#6129 = CARTESIAN_POINT ( 'NONE',  ( 2.862020680886599333, -72.79547149457074795, 4.100960146803977580 ) ) ;
#6130 = CARTESIAN_POINT ( 'NONE',  ( 4.037591185471440802, -62.70452850542925916, -5.718994135553947977 ) ) ;
#6131 = ORIENTED_EDGE ( 'NONE', *, *, #1253, .T. ) ;
#6132 = ADVANCED_FACE ( 'NONE', ( #3451 ), #6727, .T. ) ;
#6133 = CARTESIAN_POINT ( 'NONE',  ( 54.99999999999999289, -1.301042606982604729E-15, 7.499999999999997335 ) ) ;
#6134 = EDGE_CURVE ( 'NONE', #3662, #7486, #6104, .T. ) ;
#6135 = EDGE_LOOP ( 'NONE', ( #2367, #262, #3475, #5116 ) ) ;
#6136 = CARTESIAN_POINT ( 'NONE',  ( -1.500000000000001110, -27.00000000000000000, 5.000000000000000000 ) ) ;
#6137 = CARTESIAN_POINT ( 'NONE',  ( 2.862020680886515400, -86.70452850542925205, -4.100960146804039752 ) ) ;
#6138 = CARTESIAN_POINT ( 'NONE',  ( 0.09506052544086046607, -79.50452850542926342, 4.999999999999997335 ) ) ;
#6139 = CARTESIAN_POINT ( 'NONE',  ( -1.719659006605372298, -75.15452850542925489, -4.969112962950015699 ) ) ;
#6140 = CARTESIAN_POINT ( 'NONE',  ( -2.882544866740857081, -83.89547149457074227, 0.8366430509619596778 ) ) ;
#6141 = CARTESIAN_POINT ( 'NONE',  ( -2.882544866740859746, -62.89547149457074227, 0.8366430509619596778 ) ) ;
#6142 = CARTESIAN_POINT ( 'NONE',  ( -5.257311121191324155, -66.75452850542923500, 0.09995255151729526277 ) ) ;
#6143 = CARTESIAN_POINT ( 'NONE',  ( -6.686770931921504513, -84.60452850542927195, -2.072711028461647675 ) ) ;
#6144 = CARTESIAN_POINT ( 'NONE',  ( -2.823794231030023028, -60.90452850542925489, 1.017458915287783316 ) ) ;
#6145 = APPLICATION_PROTOCOL_DEFINITION ( 'draft international standard', 'automotive_design', 1998, #2292 ) ;
#6146 = ORIENTED_EDGE ( 'NONE', *, *, #3794, .F. ) ;
#6147 = LINE ( 'NONE', #6659, #6174 ) ;
#6148 = PRODUCT_DEFINITION_SHAPE ( 'NONE', 'NONE',  #8341 ) ;
#6149 = VERTEX_POINT ( 'NONE', #3020 ) ;
#6150 = CARTESIAN_POINT ( 'NONE',  ( -5.999999999999988454, -100.0010000000000048, 2.500000000000000888 ) ) ;
#6151 = CARTESIAN_POINT ( 'NONE',  ( 3.154386672714807549, -68.25452850542924921, -0.09995255151727241993 ) ) ;
#6152 = CARTESIAN_POINT ( 'NONE',  ( -7.360235569667858968, -80.74547149457075079, -0.09995255151716124498 ) ) ;
#6153 = DIRECTION ( 'NONE',  ( -0.000000000000000000, -0.000000000000000000, -1.000000000000000000 ) ) ;
#6154 =( REPRESENTATION_RELATIONSHIP ('NONE','NONE', #4188, #1613 ) REPRESENTATION_RELATIONSHIP_WITH_TRANSFORMATION ( #863 )SHAPE_REPRESENTATION_RELATIONSHIP( ) );
#6155 = CARTESIAN_POINT ( 'NONE',  ( 54.99999999999999289, 50.00000000000000000, -7.500000000000000000 ) ) ;
#6156 = CARTESIAN_POINT ( 'NONE',  ( 2.610703060766984329, -82.95452850542925205, 1.773238653441072232 ) ) ;
#6157 = VECTOR ( 'NONE', #7901, 1000.000000000000000 ) ;
#6158 = ADVANCED_FACE ( 'NONE', ( #2432 ), #2938, .F. ) ;
#6159 = FILL_AREA_STYLE_COLOUR ( '', #2879 ) ;
#6160 = ORIENTED_EDGE ( 'NONE', *, *, #1781, .T. ) ;
#6161 = DIRECTION ( 'NONE',  ( -9.251858538542971581E-17, 1.000000000000000000, 0.000000000000000000 ) ) ;
#6162 = CARTESIAN_POINT ( 'NONE',  ( 1.069819614139559061, -94.65452850542924068, 2.969112962950023249 ) ) ;
#6163 = CARTESIAN_POINT ( 'NONE',  ( 2.369498399071076733, -70.84547149457073090, -6.969112962950057444 ) ) ;
#6164 = ORIENTED_EDGE ( 'NONE', *, *, #7782, .T. ) ;
#6165 = CARTESIAN_POINT ( 'NONE',  ( 2.862020680886599333, -78.79547149457074795, 4.100960146803977580 ) ) ;
#6166 = CARTESIAN_POINT ( 'NONE',  ( 4.725907263620372056, -67.09547149457073090, 1.635492904037598283 ) ) ;
#6167 = CARTESIAN_POINT ( 'NONE',  ( -4.784657899331191011, -69.60452850542925773, -1.454677039711773867 ) ) ;
#6168 = CARTESIAN_POINT ( 'NONE',  ( -1.500000000000001110, -27.00000000000000000, -2.499999999999999556 ) ) ;
#6169 = CARTESIAN_POINT ( 'NONE',  ( -4.194503406049384431, -62.44547149457072521, -3.171033256558012159 ) ) ;
#6170 = PRESENTATION_STYLE_ASSIGNMENT (( #518 ) ) ;
#6171 = CARTESIAN_POINT ( 'NONE',  ( 6.686770931921522276, -59.10452850542926484, 2.072711028461649008 ) ) ;
#6172 = VERTEX_POINT ( 'NONE', #4994 ) ;
#6173 = VECTOR ( 'NONE', #1399, 1000.000000000000000 ) ;
#6174 = VECTOR ( 'NONE', #6617, 1000.000000000000000 ) ;
#6175 = LINE ( 'NONE', #402, #3161 ) ;
#6176 = AXIS2_PLACEMENT_3D ( 'NONE', #33, #708, #7845 ) ;
#6177 = ORIENTED_EDGE ( 'NONE', *, *, #226, .F. ) ;
#6178 = AXIS2_PLACEMENT_3D ( 'NONE', #3924, #3881, #757 ) ;
#6179 = CARTESIAN_POINT ( 'NONE',  ( -47.50000000000002132, -97.00000000000000000, -12.50000000000002309 ) ) ;
#6180 = CARTESIAN_POINT ( 'NONE',  ( 3.015831842038235955, -91.80452850542926058, 3.989209796945429432 ) ) ;
#6181 = CARTESIAN_POINT ( 'NONE',  ( 4.784657899331210551, -80.10452850542925773, 1.454677039711774533 ) ) ;
#6182 = CARTESIAN_POINT ( 'NONE',  ( -0.09506052544084224454, -60.00452850542925631, -4.999999999999997335 ) ) ;
#6183 = CARTESIAN_POINT ( 'NONE',  ( 1.840261337453221291, -85.69547149457073942, -2.371175808195584267 ) ) ;
#6184 = CARTESIAN_POINT ( 'NONE',  ( -1.686450176301619308, -59.29547149457074084, -2.482926158054096000 ) ) ;
#6185 = CARTESIAN_POINT ( 'NONE',  ( 3.015831842038233290, -70.80452850542926058, 3.989209796945429432 ) ) ;
#6186 = CARTESIAN_POINT ( 'NONE',  ( 4.037591185471444355, -86.70452850542925205, -5.718994135553947977 ) ) ;
#6187 = CARTESIAN_POINT ( 'NONE',  ( 1.840261337453222845, -97.69547149457076785, -2.371175808195584267 ) ) ;
#6188 = ORIENTED_EDGE ( 'NONE', *, *, #8275, .T. ) ;
#6189 = DIRECTION ( 'NONE',  ( -0.000000000000000000, -0.000000000000000000, -1.000000000000000000 ) ) ;
#6190 =( GEOMETRIC_REPRESENTATION_CONTEXT ( 3 ) GLOBAL_UNCERTAINTY_ASSIGNED_CONTEXT ( ( #979 ) ) GLOBAL_UNIT_ASSIGNED_CONTEXT ( ( #1240, #8318, #2588 ) ) REPRESENTATION_CONTEXT ( 'NONE', 'WORKASPACE' ) );
#6191 = ORIENTED_EDGE ( 'NONE', *, *, #7652, .F. ) ;
#6192 = CARTESIAN_POINT ( 'NONE',  ( 4.194503406049340022, -92.55452850542924637, -3.171033256558100977 ) ) ;
#6193 = CARTESIAN_POINT ( 'NONE',  ( -2.610703060766966122, -69.45452850542925205, -1.773238653441072232 ) ) ;
#6194 = CARTESIAN_POINT ( 'NONE',  ( 6.686770931921477867, -76.39547149457074227, -2.072711028461788896 ) ) ;
#6195 = CARTESIAN_POINT ( 'NONE',  ( -4.725907263620319654, -90.90452850542926910, 1.635492904037698647 ) ) ;
#6196 = EDGE_CURVE ( 'NONE', #5382, #8240, #8086, .T. ) ;
#6197 = CARTESIAN_POINT ( 'NONE',  ( -4.725907263620350740, -95.59547149457074511, -1.635492904037597617 ) ) ;
#6198 = CARTESIAN_POINT ( 'NONE',  ( 0.09506052544083994083, -85.50452850542926342, 2.999999999999997780 ) ) ;
#6199 = EDGE_CURVE ( 'NONE', #5781, #1490, #6807, .T. ) ;
#6200 = CARTESIAN_POINT ( 'NONE',  ( 80.00000000000000000, -1.734723475976807094E-15, 12.50000000000000000 ) ) ;
#6201 = ORIENTED_EDGE ( 'NONE', *, *, #6889, .F. ) ;
#6202 = DIRECTION ( 'NONE',  ( 0.000000000000000000, 0.000000000000000000, -1.000000000000000000 ) ) ;
#6203 = CARTESIAN_POINT ( 'NONE',  ( -1.529537955723671905, -61.35452850542925773, 5.030887037049979860 ) ) ;
#6204 = CARTESIAN_POINT ( 'NONE',  ( -6.686770931921459216, -71.89547149457074227, 2.072711028461789784 ) ) ;
#6205 =( NAMED_UNIT ( * ) PLANE_ANGLE_UNIT ( ) SI_UNIT ( $, .RADIAN. ) );
#6206 = CARTESIAN_POINT ( 'NONE',  ( 5.186942113755784511, -97.00000000000001421, 1.679816887229922839 ) ) ;
#6207 = CARTESIAN_POINT ( 'NONE',  ( 1.719659006605285034, -70.84547149457074511, -4.969112962950050338 ) ) ;
#6208 = CARTESIAN_POINT ( 'NONE',  ( -3.015831842038129817, -72.19547149457073942, 3.989209796945492048 ) ) ;
#6209 = CARTESIAN_POINT ( 'NONE',  ( -0.09506052544081705635, -93.00452850542926342, -2.999999999999997780 ) ) ;
#6210 = CARTESIAN_POINT ( 'NONE',  ( 45.00000000000000000, -14.99999999999999289, 4.499999999999999112 ) ) ;
#6211 = CARTESIAN_POINT ( 'NONE',  ( -3.015831842038216415, -66.30452850542926058, -3.989209796945429432 ) ) ;
#6212 = CARTESIAN_POINT ( 'NONE',  ( 2.179377348189632357, -96.64547149457075648, 7.030887037049939003 ) ) ;
#6213 = CARTESIAN_POINT ( 'NONE',  ( -0.09506052544083808120, -93.00452850542926342, -4.999999999999997335 ) ) ;
#6214 = ORIENTED_EDGE ( 'NONE', *, *, #2242, .T. ) ;
#6215 = UNCERTAINTY_MEASURE_WITH_UNIT (LENGTH_MEASURE( 1.000000000000000082E-05 ), #4015, 'distance_accuracy_value', 'NONE');
#6216 = CARTESIAN_POINT ( 'NONE',  ( -3.989863994746656317E-14, -97.00000000000000000, -4.999999999999997335 ) ) ;
#6217 = PRODUCT ( 'pin', 'pin', '', ( #8280 ) ) ;
#6218 = EDGE_CURVE ( 'NONE', #1800, #6969, #6932, .T. ) ;
#6219 = ORIENTED_EDGE ( 'NONE', *, *, #7387, .F. ) ;
#6220 = LINE ( 'NONE', #6179, #2748 ) ;
#6221 = CARTESIAN_POINT ( 'NONE',  ( 4.312004677471078296, -88.95452850542922363, 3.009306630940844496 ) ) ;
#6222 = CARTESIAN_POINT ( 'NONE',  ( 4.725907263620374721, -91.09547149457074511, 1.635492904037598283 ) ) ;
#6223 = CARTESIAN_POINT ( 'NONE',  ( -0.09506052544084186984, -63.00452850542925631, -4.999999999999997335 ) ) ;
#6224 = VECTOR ( 'NONE', #2543, 1000.000000000000000 ) ;
#6225 = CARTESIAN_POINT ( 'NONE',  ( 2.823794231030060331, -79.09547149457075932, 1.017458915287723809 ) ) ;
#6226 = CARTESIAN_POINT ( 'NONE',  ( 4.784657899331179465, -91.39547149457075648, -1.454677039711874009 ) ) ;
#6227 = CARTESIAN_POINT ( 'NONE',  ( 4.725907263620340082, -65.40452850542925489, -1.635492904037697981 ) ) ;
#6228 = CARTESIAN_POINT ( 'NONE',  ( -6.013306294175152722, -75.45452850542925205, -4.245374608440613429 ) ) ;
#6229 = CARTESIAN_POINT ( 'NONE',  ( 1.686450176301638182, -93.79547149457076216, 2.482926158054096000 ) ) ;
#6230 = PRODUCT_RELATED_PRODUCT_CATEGORY ( 'part', '', ( #3131 ) ) ;
#6231 = VERTEX_POINT ( 'NONE', #5660 ) ;
#6232 = PLANE ( 'NONE',  #4413 ) ;
#6233 = CARTESIAN_POINT ( 'NONE',  ( 4.784657899331211439, -92.10452850542925773, 1.454677039711774533 ) ) ;
#6234 = CARTESIAN_POINT ( 'NONE',  ( -1.840261337453252155, -72.30452850542926058, -2.371175808195547852 ) ) ;
#6235 = CARTESIAN_POINT ( 'NONE',  ( -7.360235569667860744, -60.75452850542924921, 0.09995255151731782806 ) ) ;
#6236 = VECTOR ( 'NONE', #4195, 1000.000000000000000 ) ;
#6237 = CARTESIAN_POINT ( 'NONE',  ( -6.013306294175058575, -84.04547149457074795, 4.245374608440741326 ) ) ;
#6238 = CARTESIAN_POINT ( 'NONE',  ( 3.015831842038236399, -94.80452850542924637, 3.989209796945429432 ) ) ;
#6239 = CARTESIAN_POINT ( 'NONE',  ( 4.784657899331179465, -91.39547149457075648, -1.454677039711874009 ) ) ;
#6240 = CARTESIAN_POINT ( 'NONE',  ( -1.069819614139536412, -90.15452850542926910, -2.969112962950023249 ) ) ;
#6241 = AXIS2_PLACEMENT_3D ( 'NONE', #2682, #4730, #2807 ) ;
#6242 = VECTOR ( 'NONE', #7382, 1000.000000000000114 ) ;
#6243 = DIRECTION ( 'NONE',  ( -1.000000000000000000, 0.000000000000000000, -0.000000000000000000 ) ) ;
#6244 = COLOUR_RGB ( '', 0.09019608, 0.27058824, 0.51372549) ;
#6245 = ORIENTED_EDGE ( 'NONE', *, *, #6341, .F. ) ;
#6246 = LINE ( 'NONE', #5683, #4094 ) ;
#6247 = CARTESIAN_POINT ( 'NONE',  ( -1.529537955723672349, -58.35452850542924352, 5.030887037049979860 ) ) ;
#6248 = CARTESIAN_POINT ( 'NONE',  ( 2.179377348189628361, -69.64547149457072805, 7.030887037049939003 ) ) ;
#6249 = FILL_AREA_STYLE ('',( #3047 ) ) ;
#6250 = CARTESIAN_POINT ( 'NONE',  ( 5.478861521945414204, -97.00000000000005684, 0.9668479938647240868 ) ) ;
#6251 = CARTESIAN_POINT ( 'NONE',  ( -4.784657899331159037, -68.89547149457074227, 1.454677039711874675 ) ) ;
#6252 = CARTESIAN_POINT ( 'NONE',  ( -1.529537955723778042, -65.14547149457074227, -5.030887037049945221 ) ) ;
#6253 = VECTOR ( 'NONE', #8123, 1000.000000000000000 ) ;
#6254 = CARTESIAN_POINT ( 'NONE',  ( -4.194503406049321370, -58.05452850542925347, 3.171033256558100533 ) ) ;
#6255 = CARTESIAN_POINT ( 'NONE',  ( 6.123233995736760366E-16, -27.00000000000000000, 4.500000000000000888 ) ) ;
#6256 = EDGE_CURVE ( 'NONE', #2910, #6149, #5544, .T. ) ;
#6257 = CARTESIAN_POINT ( 'NONE',  ( -4.312004677471057867, -72.45452850542922363, -3.009306630940844052 ) ) ;
#6258 = EDGE_CURVE ( 'NONE', #1341, #4394, #483, .T. ) ;
#6259 = CARTESIAN_POINT ( 'NONE',  ( -1.529537955723778486, -62.14547149457074227, -5.030887037049945221 ) ) ;
#6260 = ORIENTED_EDGE ( 'NONE', *, *, #5522, .T. ) ;
#6261 = CLOSED_SHELL ( 'NONE', ( #1589, #4700, #3945, #4333, #3654 ) ) ;
#6262 = PLANE ( 'NONE',  #2091 ) ;
#6263 = EDGE_CURVE ( 'NONE', #3327, #8040, #6220, .T. ) ;
#6264 = VERTEX_POINT ( 'NONE', #404 ) ;
#6265 = CARTESIAN_POINT ( 'NONE',  ( -0.09506052544083767875, -96.00452850542926342, -4.999999999999997335 ) ) ;
#6266 = CARTESIAN_POINT ( 'NONE',  ( -1.719659006605371854, -78.15452850542925489, -4.969112962950016588 ) ) ;
#6267 = CARTESIAN_POINT ( 'NONE',  ( -3.015831842038127153, -90.19547149457073942, 3.989209796945492048 ) ) ;
#6268 = CARTESIAN_POINT ( 'NONE',  ( -4.725907263620324095, -57.90452850542925489, 1.635492904037698647 ) ) ;
#6269 = CARTESIAN_POINT ( 'NONE',  ( -2.493201789345290464, -83.44547149457073942, -1.934965279058240561 ) ) ;
#6270 = CARTESIAN_POINT ( 'NONE',  ( -6.013306294175152722, -75.45452850542925205, -4.245374608440613429 ) ) ;
#6271 = CARTESIAN_POINT ( 'NONE',  ( -4.194503406049383543, -83.44547149457071100, -3.171033256558012159 ) ) ;
#6272 = CARTESIAN_POINT ( 'NONE',  ( -4.312004677471060532, -63.45452850542926626, -3.009306630940844052 ) ) ;
#6273 = CARTESIAN_POINT ( 'NONE',  ( 7.360235569667877620, -74.25452850542924921, -0.09995255151731691212 ) ) ;
#6274 = CARTESIAN_POINT ( 'NONE',  ( 0.09506052544077819855, -91.99547149457075079, -2.999999999999997780 ) ) ;
#6275 = ORIENTED_EDGE ( 'NONE', *, *, #611, .T. ) ;
#6276 = LINE ( 'NONE', #2404, #5500 ) ;
#6277 = FACE_OUTER_BOUND ( 'NONE', #773, .T. ) ;
#6278 = ORIENTED_EDGE ( 'NONE', *, *, #374, .T. ) ;
#6279 = CARTESIAN_POINT ( 'NONE',  ( 5.257311121191343695, -89.25452850542923500, -0.09995255151729466603 ) ) ;
#6280 = CARTESIAN_POINT ( 'NONE',  ( -2.610703060766966566, -66.45452850542925205, -1.773238653441072232 ) ) ;
#6281 = CARTESIAN_POINT ( 'NONE',  ( 1.719659006605392504, -91.65452850542925489, 4.969112962950016588 ) ) ;
#6282 = CARTESIAN_POINT ( 'NONE',  ( 0.09506052544073390065, -73.99547149457075079, -6.999999999999997335 ) ) ;
#6283 = CARTESIAN_POINT ( 'NONE',  ( 4.784657899331211439, -92.10452850542925773, 1.454677039711774533 ) ) ;
#6284 = CARTESIAN_POINT ( 'NONE',  ( 4.312004677471013459, -82.54547149457073374, -3.009306630940932425 ) ) ;
#6285 = CARTESIAN_POINT ( 'NONE',  ( -0.09506052544081930455, -75.00452850542926342, -2.999999999999997780 ) ) ;
#6286 = DIRECTION ( 'NONE',  ( 0.000000000000000000, 1.000000000000000000, 0.000000000000000000 ) ) ;
#6287 = ORIENTED_EDGE ( 'NONE', *, *, #6316, .F. ) ;
#6288 = ADVANCED_FACE ( 'NONE', ( #3566 ), #361, .T. ) ;
#6289 =( NAMED_UNIT ( * ) PLANE_ANGLE_UNIT ( ) SI_UNIT ( $, .RADIAN. ) );
#6290 = CARTESIAN_POINT ( 'NONE',  ( -0.8796985632578772085, -94.35452850542925773, 3.030887037049973198 ) ) ;
#6291 = CARTESIAN_POINT ( 'NONE',  ( 4.191402346623077868, -73.69547149457073942, -5.607243785695398941 ) ) ;
#6292 = DIRECTION ( 'NONE',  ( 0.000000000000000000, 0.000000000000000000, 1.000000000000000000 ) ) ;
#6293 = CARTESIAN_POINT ( 'NONE',  ( 4.312004677471009906, -64.54547149457073374, -3.009306630940932425 ) ) ;
#6294 = CARTESIAN_POINT ( 'NONE',  ( -4.312004677470994807, -63.04547149457074084, 3.009306630940933758 ) ) ;
#6295 = CARTESIAN_POINT ( 'NONE',  ( -3.015831842038216859, -60.30452850542926058, -3.989209796945429432 ) ) ;
#6296 = CARTESIAN_POINT ( 'NONE',  ( 95.11234224026316042, -49.99999999999999289, -20.00000000000000000 ) ) ;
#6297 = VECTOR ( 'NONE', #3306, 1000.000000000000000 ) ;
#6298 = CARTESIAN_POINT ( 'NONE',  ( -5.257311121191324155, -66.75452850542923500, 0.09995255151729526277 ) ) ;
#6299 = CARTESIAN_POINT ( 'NONE',  ( 0.09506052544073689825, -97.99547149457075079, -6.999999999999997335 ) ) ;
#6300 = ORIENTED_EDGE ( 'NONE', *, *, #3379, .T. ) ;
#6301 = CARTESIAN_POINT ( 'NONE',  ( -80.00000000000000000, -19.99999999999999645, -12.50000000000000355 ) ) ;
#6302 = EDGE_CURVE ( 'NONE', #2454, #3855, #7999, .T. ) ;
#6303 = ORIENTED_EDGE ( 'NONE', *, *, #5184, .F. ) ;
#6304 = DIRECTION ( 'NONE',  ( 0.000000000000000000, 0.000000000000000000, 1.000000000000000000 ) ) ;
#6305 = CARTESIAN_POINT ( 'NONE',  ( -2.862020680886493640, -82.20452850542925205, 4.100960146804039752 ) ) ;
#6306 = CARTESIAN_POINT ( 'NONE',  ( -2.862020680886579349, -86.29547149457074795, -4.100960146803977580 ) ) ;
#6307 = CARTESIAN_POINT ( 'NONE',  ( 4.784657899331207886, -62.10452850542925063, 1.454677039711774533 ) ) ;
#6308 = CARTESIAN_POINT ( 'NONE',  ( -1.840261337453201529, -69.19547149457073942, 2.371175808195584267 ) ) ;
#6309 = AXIS2_PLACEMENT_3D ( 'NONE', #4127, #2791, #2284 ) ;
#6310 = CARTESIAN_POINT ( 'NONE',  ( -2.179377348189461827, -76.35452850542924352, 7.030887037049988741 ) ) ;
#6311 = CARTESIAN_POINT ( 'NONE',  ( -1.719659006605264162, -90.34547149457074511, 4.969112962950051227 ) ) ;
#6312 = CARTESIAN_POINT ( 'NONE',  ( 1.529537955723688780, -62.85452850542925063, -5.030887037049978971 ) ) ;
#6313 = CARTESIAN_POINT ( 'NONE',  ( 4.037591185471442579, -77.70452850542925205, -5.718994135553947977 ) ) ;
#6314 = PRODUCT_DEFINITION_FORMATION_WITH_SPECIFIED_SOURCE ( 'ANY', '', #4875, .NOT_KNOWN. ) ;
#6315 = CARTESIAN_POINT ( 'NONE',  ( -2.493201789345290020, -86.44547149457073942, -1.934965279058240561 ) ) ;
#6316 = EDGE_CURVE ( 'NONE', #5555, #1673, #1081, .T. ) ;
#6317 = ORIENTED_EDGE ( 'NONE', *, *, #6814, .F. ) ;
#6318 = APPLICATION_CONTEXT ( 'automotive_design' ) ;
#6319 = DIRECTION ( 'NONE',  ( -1.000000000000000000, 0.000000000000000000, 0.000000000000000000 ) ) ;
#6320 = DIRECTION ( 'NONE',  ( 1.000000000000000000, 0.000000000000000000, 0.000000000000000000 ) ) ;
#6321 = ORIENTED_EDGE ( 'NONE', *, *, #2308, .F. ) ;
#6322 = CARTESIAN_POINT ( 'NONE',  ( -3.015831842038213750, -90.30452850542926058, -3.989209796945429432 ) ) ;
#6323 = CARTESIAN_POINT ( 'NONE',  ( 0.09506052544083691547, -61.50452850542925631, 2.999999999999997780 ) ) ;
#6324 = COLOUR_RGB ( '', 0.40784314, 0.44705882, 0.49803922) ;
#6325 = CARTESIAN_POINT ( 'NONE',  ( 2.862020680886516288, -92.70452850542926626, -4.100960146804039752 ) ) ;
#6326 = CARTESIAN_POINT ( 'NONE',  ( 6.628020296210686446, -70.09547149457073090, 2.253526892787472757 ) ) ;
#6327 = CARTESIAN_POINT ( 'NONE',  ( 4.725907263620374721, -88.09547149457074511, 1.635492904037598283 ) ) ;
#6328 = CARTESIAN_POINT ( 'NONE',  ( -3.154386672714789785, -75.75452850542926342, 0.09995255151727280851 ) ) ;
#6329 = VECTOR ( 'NONE', #781, 1000.000000000000000 ) ;
#6330 = CARTESIAN_POINT ( 'NONE',  ( 6.123233995736760366E-16, -27.00000000000000000, 4.500000000000000888 ) ) ;
#6331 = ORIENTED_EDGE ( 'NONE', *, *, #2092, .F. ) ;
#6332 = EDGE_CURVE ( 'NONE', #6231, #4020, #2978, .T. ) ;
#6333 = CARTESIAN_POINT ( 'NONE',  ( 0.8796985632578997460, -83.85452850542927195, -3.030887037049972310 ) ) ;
#6334 = CARTESIAN_POINT ( 'NONE',  ( -6.628020296210667794, -71.59547149457071669, -2.253526892787471869 ) ) ;
#6335 = CARTESIAN_POINT ( 'NONE',  ( -47.50000000000000711, -54.00000000000000711, 12.50000000000001954 ) ) ;
#6336 = CARTESIAN_POINT ( 'NONE',  ( -5.257311121191325043, -68.74547149457073658, -0.09995255151718372699 ) ) ;
#6337 = CARTESIAN_POINT ( 'NONE',  ( -7.360235569667856304, -95.74547149457073658, -0.09995255151716124498 ) ) ;
#6338 = CARTESIAN_POINT ( 'NONE',  ( -0.09506052544081666777, -96.00452850542926342, -2.999999999999997780 ) ) ;
#6339 = PLANE ( 'NONE',  #6912 ) ;
#6340 = CARTESIAN_POINT ( 'NONE',  ( 2.862020680886513180, -68.70452850542925205, -4.100960146804039752 ) ) ;
#6341 = EDGE_CURVE ( 'NONE', #200, #4272, #1120, .T. ) ;
#6342 = CARTESIAN_POINT ( 'NONE',  ( -5.895805022753475733, -95.44547149457075363, -4.407101234057782868 ) ) ;
#6343 = ORIENTED_EDGE ( 'NONE', *, *, #5114, .T. ) ;
#6344 = EDGE_CURVE ( 'NONE', #4707, #6384, #4476, .T. ) ;
#6345 = PLANE ( 'NONE',  #5983 ) ;
#6346 = PRODUCT_CONTEXT ( 'NONE', #2019, 'mechanical' ) ;
#6347 = ORIENTED_EDGE ( 'NONE', *, *, #2795, .F. ) ;
#6348 = FACE_OUTER_BOUND ( 'NONE', #2029, .T. ) ;
#6349 = CARTESIAN_POINT ( 'NONE',  ( 0.09506052544086007750, -76.50452850542924921, 4.999999999999997335 ) ) ;
#6350 = CARTESIAN_POINT ( 'NONE',  ( -4.784657899331156372, -92.89547149457075648, 1.454677039711874675 ) ) ;
#6351 = CARTESIAN_POINT ( 'NONE',  ( -3.015831842038217303, -57.30452850542925347, -3.989209796945429432 ) ) ;
#6352 = CARTESIAN_POINT ( 'NONE',  ( -2.823794231030041235, -68.59547149457073090, -1.017458915287723364 ) ) ;
#6353 = CARTESIAN_POINT ( 'NONE',  ( 4.037591185471442579, -74.70452850542925205, -5.718994135553947977 ) ) ;
#6354 = CARTESIAN_POINT ( 'NONE',  ( -4.725907263620352516, -86.59547149457075932, -1.635492904037597617 ) ) ;
#6355 = CARTESIAN_POINT ( 'NONE',  ( -2.862020680886496748, -58.20452850542925916, 4.100960146804039752 ) ) ;
#6356 = ADVANCED_FACE ( 'NONE', ( #4918, #3734, #4951 ), #5620, .F. ) ;
#6357 = CARTESIAN_POINT ( 'NONE',  ( -6.628020296210620721, -78.90452850542925489, 2.253526892787613978 ) ) ;
#6358 = CARTESIAN_POINT ( 'NONE',  ( -3.154386672714787565, -92.74547149457073658, -0.09995255151720625064 ) ) ;
#6359 = ORIENTED_EDGE ( 'NONE', *, *, #3773, .T. ) ;
#6360 = CARTESIAN_POINT ( 'NONE',  ( 1.500000000000002442, -27.00000000000000000, 5.000000000000000000 ) ) ;
#6361 = DIRECTION ( 'NONE',  ( -0.000000000000000000, -0.000000000000000000, -1.000000000000000000 ) ) ;
#6362 = PRODUCT_DEFINITION_SHAPE ( 'NONE', 'NONE',  #1392 ) ;
#6363 = ORIENTED_EDGE ( 'NONE', *, *, #2626, .T. ) ;
#6364 = CARTESIAN_POINT ( 'NONE',  ( -4.312004677471056091, -90.45452850542926626, -3.009306630940843608 ) ) ;
#6365 = CARTESIAN_POINT ( 'NONE',  ( 1.069819614139554842, -58.65452850542925489, 2.969112962950023249 ) ) ;
#6366 = CARTESIAN_POINT ( 'NONE',  ( 7.360235569667875843, -59.25452850542926342, -0.09995255151731691212 ) ) ;
#6367 = CARTESIAN_POINT ( 'NONE',  ( -6.686770931921460992, -65.89547149457074227, 2.072711028461789784 ) ) ;
#6368 = CARTESIAN_POINT ( 'NONE',  ( -2.862020680886579349, -89.29547149457074795, -4.100960146803977580 ) ) ;
#6369 = CARTESIAN_POINT ( 'NONE',  ( 1.840261337453270807, -76.80452850542926058, 2.371175808195547852 ) ) ;
#6370 = DIRECTION ( 'NONE',  ( 0.000000000000000000, 0.000000000000000000, 1.000000000000000000 ) ) ;
#6371 = CARTESIAN_POINT ( 'NONE',  ( 1.686450176301586668, -86.70452850542925205, -2.482926158054133303 ) ) ;
#6372 = CARTESIAN_POINT ( 'NONE',  ( 4.191402346623076980, -61.69547149457074653, -5.607243785695398941 ) ) ;
#6373 = CARTESIAN_POINT ( 'NONE',  ( 5.283807651323763288, -96.99999999999990052, -2.555618791970358572 ) ) ;
#6374 = CARTESIAN_POINT ( 'NONE',  ( -0.09506052544073617661, -69.49547149457075079, 4.999999999999997335 ) ) ;
#6375 = CARTESIAN_POINT ( 'NONE',  ( 2.179377348189632357, -96.64547149457075648, 7.030887037049939003 ) ) ;
#6376 = CARTESIAN_POINT ( 'NONE',  ( 3.015831842038231958, -58.80452850542925347, 3.989209796945429432 ) ) ;
#6377 = DIRECTION ( 'NONE',  ( 0.000000000000000000, 0.000000000000000000, -1.000000000000000000 ) ) ;
#6378 = VECTOR ( 'NONE', #703, 1000.000000000000000 ) ;
#6379 = VECTOR ( 'NONE', #6161, 1000.000000000000000 ) ;
#6380 = CARTESIAN_POINT ( 'NONE',  ( 1.529537955723689002, -65.85452850542924352, -5.030887037049978971 ) ) ;
#6381 = CARTESIAN_POINT ( 'NONE',  ( -4.191402346623055664, -93.19547149457075363, 5.607243785695398941 ) ) ;
#6382 = VECTOR ( 'NONE', #6631, 1000.000000000000000 ) ;
#6383 =( NAMED_UNIT ( * ) PLANE_ANGLE_UNIT ( ) SI_UNIT ( $, .RADIAN. ) );
#6384 = VERTEX_POINT ( 'NONE', #6265 ) ;
#6385 = DIRECTION ( 'NONE',  ( -0.000000000000000000, 1.000000000000000000, 2.775557561562891351E-16 ) ) ;
#6386 = EDGE_CURVE ( 'NONE', #6524, #2779, #2473, .T. ) ;
#6387 = VERTEX_POINT ( 'NONE', #443 ) ;
#6388 = FACE_OUTER_BOUND ( 'NONE', #2200, .T. ) ;
#6389 = CARTESIAN_POINT ( 'NONE',  ( -0.09506052544083998246, -78.00452850542926342, -4.999999999999997335 ) ) ;
#6390 = CARTESIAN_POINT ( 'NONE',  ( -4.194503406049383543, -86.44547149457071100, -3.171033256558012159 ) ) ;
#6391 = ADVANCED_FACE ( 'NONE', ( #8163 ), #5036, .F. ) ;
#6392 = CARTESIAN_POINT ( 'NONE',  ( 4.306376502030560438, -96.99999999999997158, 1.631842557598098375 ) ) ;
#6393 = CARTESIAN_POINT ( 'NONE',  ( 1.069819614139494002, -73.84547149457073090, -2.969112962950042789 ) ) ;
#6394 = CARTESIAN_POINT ( 'NONE',  ( 4.037591185471443467, -80.70452850542925205, -5.718994135553947977 ) ) ;
#6395 = CARTESIAN_POINT ( 'NONE',  ( 4.194503406049402194, -87.94547149457072521, 3.171033256558012159 ) ) ;
#6396 = CARTESIAN_POINT ( 'NONE',  ( 2.862020680886511848, -59.70452850542925205, -4.100960146804039752 ) ) ;
#6397 = CARTESIAN_POINT ( 'NONE',  ( 6.686770931921523164, -74.10452850542924352, 2.072711028461649008 ) ) ;
#6398 = CARTESIAN_POINT ( 'NONE',  ( 3.154386672714809770, -85.24547149457075079, 0.09995255151720662534 ) ) ;
#6399 = ORIENTED_EDGE ( 'NONE', *, *, #407, .T. ) ;
#6400 = PLANE ( 'NONE',  #8328 ) ;
#6401 = LINE ( 'NONE', #579, #3815 ) ;
#6402 = VERTEX_POINT ( 'NONE', #60 ) ;
#6403 = CARTESIAN_POINT ( 'NONE',  ( -3.015831842038214194, -81.30452850542926058, -3.989209796945429432 ) ) ;
#6404 = CARTESIAN_POINT ( 'NONE',  ( -0.8796985632578812053, -61.35452850542925773, 3.030887037049973198 ) ) ;
#6405 = ADVANCED_BREP_SHAPE_REPRESENTATION ( '', ( #1832, #2840 ), #4982 ) ;
#6406 = CARTESIAN_POINT ( 'NONE',  ( -6.686770931921507177, -60.60452850542926484, -2.072711028461647675 ) ) ;
#6407 = CARTESIAN_POINT ( 'NONE',  ( -5.895805022753477509, -74.44547149457072521, -4.407101234057782868 ) ) ;
#6408 = CARTESIAN_POINT ( 'NONE',  ( -0.09506052544073352595, -90.49547149457073658, 4.999999999999997335 ) ) ;
#6409 = CARTESIAN_POINT ( 'NONE',  ( 1.069819614139556840, -73.65452850542925489, 2.969112962950023249 ) ) ;
#6410 = LINE ( 'NONE', #170, #6718 ) ;
#6411 = CARTESIAN_POINT ( 'NONE',  ( 2.610703060766984773, -85.95452850542925205, 1.773238653441072232 ) ) ;
#6412 = CARTESIAN_POINT ( 'NONE',  ( 4.037591185471560706, -60.79547149457074084, 5.718994135553860936 ) ) ;
#6413 = CARTESIAN_POINT ( 'NONE',  ( 50.00000000000000000, -1.734723475976807094E-15, 12.50000000000000000 ) ) ;
#6414 = CARTESIAN_POINT ( 'NONE',  ( -4.725907263620355181, -65.59547149457073090, -1.635492904037597617 ) ) ;
#6415 = CARTESIAN_POINT ( 'NONE',  ( 3.015831842038146693, -61.69547149457073942, -3.989209796945492048 ) ) ;
#6416 = CARTESIAN_POINT ( 'NONE',  ( -5.999999999999993783, -51.00000000000000711, 2.500000000000000888 ) ) ;
#6417 = LINE ( 'NONE', #1279, #6224 ) ;
#6418 = EDGE_CURVE ( 'NONE', #8028, #6172, #4892, .T. ) ;
#6419 = CARTESIAN_POINT ( 'NONE',  ( 1.529537955723688780, -62.85452850542925063, -5.030887037049978971 ) ) ;
#6420 = CARTESIAN_POINT ( 'NONE',  ( -6.013306294175058575, -93.04547149457074795, 4.245374608440741326 ) ) ;
#6421 = FILL_AREA_STYLE_COLOUR ( '', #5253 ) ;
#6422 = EDGE_LOOP ( 'NONE', ( #2365, #4371 ) ) ;
#6423 = CARTESIAN_POINT ( 'NONE',  ( 6.123233995736760366E-16, -27.00000000000000000, -2.499999999999999556 ) ) ;
#6424 = SHAPE_DEFINITION_REPRESENTATION ( #6362, #1933 ) ;
#6425 = AXIS2_PLACEMENT_3D ( 'NONE', #299, #2876, #5443 ) ;
#6426 = DIRECTION ( 'NONE',  ( 1.000000000000000000, 9.251858538542971828E-16, -0.000000000000000000 ) ) ;
#6427 = CARTESIAN_POINT ( 'NONE',  ( 4.784657899331209663, -74.10452850542925773, 1.454677039711774533 ) ) ;
#6428 = CARTESIAN_POINT ( 'NONE',  ( -1.529537955723776488, -83.14547149457071384, -5.030887037049945221 ) ) ;
#6429 = CARTESIAN_POINT ( 'NONE',  ( 4.227511635438607307, -96.99999999999997158, 2.381263360235327919 ) ) ;
#6430 = CARTESIAN_POINT ( 'NONE',  ( -2.823794231030041235, -71.59547149457071669, -1.017458915287723364 ) ) ;
#6431 = CARTESIAN_POINT ( 'NONE',  ( -4.191402346623180009, -69.30452850542926058, -5.607243785695311900 ) ) ;
#6432 = CARTESIAN_POINT ( 'NONE',  ( 4.194503406049402194, -78.94547149457071100, 3.171033256558012159 ) ) ;
#6433 = CARTESIAN_POINT ( 'NONE',  ( 1.500000000000002665, -27.00000000000000000, 4.500000000000000888 ) ) ;
#6434 = CARTESIAN_POINT ( 'NONE',  ( -80.00000000000000000, -19.99999999999999645, -12.50000000000000000 ) ) ;
#6435 = CARTESIAN_POINT ( 'NONE',  ( -5.895805022753386027, -73.05452850542926058, 4.407101234057909878 ) ) ;
#6436 = CARTESIAN_POINT ( 'NONE',  ( -2.823794231030038571, -89.59547149457074511, -1.017458915287723364 ) ) ;
#6437 = ORIENTED_EDGE ( 'NONE', *, *, #5149, .F. ) ;
#6438 = CARTESIAN_POINT ( 'NONE',  ( -4.481820730511953954E-14, -57.99999999999999289, -4.999999999999997335 ) ) ;
#6439 = CARTESIAN_POINT ( 'NONE',  ( -5.999999999999992895, -50.00000000000000000, 2.500000000000000888 ) ) ;
#6440 = CARTESIAN_POINT ( 'NONE',  ( -4.784657899331190123, -84.60452850542927195, -1.454677039711773867 ) ) ;
#6441 = ORIENTED_EDGE ( 'NONE', *, *, #8026, .F. ) ;
#6442 = CARTESIAN_POINT ( 'NONE',  ( -4.312004677471056979, -84.45452850542923784, -3.009306630940843608 ) ) ;
#6443 = CARTESIAN_POINT ( 'NONE',  ( 0.09506052544083654077, -58.50452850542925631, 2.999999999999997780 ) ) ;
#6444 =( NAMED_UNIT ( * ) PLANE_ANGLE_UNIT ( ) SI_UNIT ( $, .RADIAN. ) );
#6445 = CARTESIAN_POINT ( 'NONE',  ( -1.529537955723669684, -82.35452850542922931, 5.030887037049979860 ) ) ;
#6446 = CARTESIAN_POINT ( 'NONE',  ( -4.037591185471545607, -71.29547149457074795, -5.718994135553860936 ) ) ;
#6447 = VECTOR ( 'NONE', #2, 1000.000000000000000 ) ;
#6448 = VECTOR ( 'NONE', #7203, 1000.000000000000000 ) ;
#6449 = CARTESIAN_POINT ( 'NONE',  ( -1.719659006605265050, -81.34547149457073090, 4.969112962950051227 ) ) ;
#6450 = CARTESIAN_POINT ( 'NONE',  ( -2.493201789345251829, -76.05452850542926058, 1.934965279058294518 ) ) ;
#6451 = DIRECTION ( 'NONE',  ( 0.000000000000000000, 0.000000000000000000, 1.000000000000000000 ) ) ;
#6452 = AXIS2_PLACEMENT_3D ( 'NONE', #5178, #5804, #7596 ) ;
#6453 = CARTESIAN_POINT ( 'NONE',  ( -3.999999999999988010, -97.00000000000000000, 4.898587196589412829E-16 ) ) ;
#6454 = CARTESIAN_POINT ( 'NONE',  ( -2.610703060766962569, -90.45452850542926626, -1.773238653441072232 ) ) ;
#6455 = CARTESIAN_POINT ( 'NONE',  ( 6.686770931921476979, -64.39547149457074227, -2.072711028461788896 ) ) ;
#6456 = EDGE_CURVE ( 'NONE', #1554, #4845, #2643, .T. ) ;
#6457 = DIRECTION ( 'NONE',  ( -0.000000000000000000, 1.000000000000000000, 1.734723475976807094E-16 ) ) ;
#6458 = CARTESIAN_POINT ( 'NONE',  ( -2.862020680886494084, -79.20452850542925205, 4.100960146804039752 ) ) ;
#6459 = CARTESIAN_POINT ( 'NONE',  ( 4.194503406049400418, -60.94547149457072521, 3.171033256558012159 ) ) ;
#6460 = DIRECTION ( 'NONE',  ( -0.000000000000000000, -0.000000000000000000, 1.000000000000000000 ) ) ;
#6461 = DIRECTION ( 'NONE',  ( 0.000000000000000000, 0.000000000000000000, -1.000000000000000000 ) ) ;
#6462 = AXIS2_PLACEMENT_3D ( 'NONE', #5161, #104, #1329 ) ;
#6463 = CARTESIAN_POINT ( 'NONE',  ( 0.09506052544085781542, -58.50452850542925631, 4.999999999999997335 ) ) ;
#6464 = CARTESIAN_POINT ( 'NONE',  ( 6.013306294175080779, -94.54547149457073374, -4.245374608440741326 ) ) ;
#6465 = VERTEX_POINT ( 'NONE', #688 ) ;
#6466 = CARTESIAN_POINT ( 'NONE',  ( -3.015831842038215527, -72.30452850542926058, -3.989209796945429432 ) ) ;
#6467 = CARTESIAN_POINT ( 'NONE',  ( 47.49999999999999289, -198.2344135219424857, -12.50000000000005151 ) ) ;
#6468 = ITEM_DEFINED_TRANSFORMATION ( 'NONE', 'NONE', #3896,  #2840 ) ;
#6469 = CARTESIAN_POINT ( 'NONE',  ( 6.123233995736760366E-16, -27.00000000000000000, -5.000000000000000000 ) ) ;
#6470 = CARTESIAN_POINT ( 'NONE',  ( -4.725907263620353405, -77.59547149457074511, -1.635492904037597617 ) ) ;
#6471 = CARTESIAN_POINT ( 'NONE',  ( -65.00000000000000000, -12.00000000000000711, 12.49999999999999822 ) ) ;
#6472 = CARTESIAN_POINT ( 'NONE',  ( 4.784657899331180353, -97.39547149457074227, -1.454677039711874009 ) ) ;
#6473 = CARTESIAN_POINT ( 'NONE',  ( 2.179377348189481367, -71.85452850542924352, -7.030887037049986077 ) ) ;
#6474 = DIRECTION ( 'NONE',  ( 1.000000000000000000, 9.251858538542971581E-17, -0.000000000000000000 ) ) ;
#6475 = CARTESIAN_POINT ( 'NONE',  ( -1.529537955723776488, -83.14547149457071384, -5.030887037049945221 ) ) ;
#6476 = CARTESIAN_POINT ( 'NONE',  ( 1.719659006605388285, -58.65452850542924068, 4.969112962950016588 ) ) ;
#6477 = CARTESIAN_POINT ( 'NONE',  ( 65.00000000000000000, -12.00000000000000355, -12.50000000000000178 ) ) ;
#6478 = CARTESIAN_POINT ( 'NONE',  ( 2.369498399071223727, -64.65452850542924068, 6.969112962950009482 ) ) ;
#6479 = CARTESIAN_POINT ( 'NONE',  ( -1.686450176301616199, -83.29547149457074795, -2.482926158054096000 ) ) ;
#6480 = ORIENTED_EDGE ( 'NONE', *, *, #6930, .T. ) ;
#6481 = DIRECTION ( 'NONE',  ( -1.000000000000000000, -0.000000000000000000, -0.000000000000000000 ) ) ;
#6482 = CARTESIAN_POINT ( 'NONE',  ( 4.784657899331211439, -92.10452850542925773, 1.454677039711774533 ) ) ;
#6483 = CARTESIAN_POINT ( 'NONE',  ( -5.257311121191322378, -90.75452850542924921, 0.09995255151729526277 ) ) ;
#6484 = EDGE_LOOP ( 'NONE', ( #6647, #6726, #6899, #8100 ) ) ;
#6485 = CARTESIAN_POINT ( 'NONE',  ( -2.862020680886493640, -82.20452850542925205, 4.100960146804039752 ) ) ;
#6486 = CARTESIAN_POINT ( 'NONE',  ( 2.823794231030062551, -97.09547149457074511, 1.017458915287723809 ) ) ;
#6487 = DIRECTION ( 'NONE',  ( 1.000000000000000000, 0.000000000000000000, 0.000000000000000000 ) ) ;
#6488 = CARTESIAN_POINT ( 'NONE',  ( 4.725907263620340970, -83.40452850542925489, -1.635492904037697981 ) ) ;
#6489 = CARTESIAN_POINT ( 'NONE',  ( -5.895805022753479285, -62.44547149457074653, -4.407101234057782868 ) ) ;
#6490 = CARTESIAN_POINT ( 'NONE',  ( -2.823794231030022583, -63.90452850542925489, 1.017458915287783316 ) ) ;
#6491 = PLANE ( 'NONE',  #7400 ) ;
#6492 = DIRECTION ( 'NONE',  ( -0.9662349396012460678, -0.2576626505603330508, 0.000000000000000000 ) ) ;
#6493 = CARTESIAN_POINT ( 'NONE',  ( 2.493201789345272257, -83.55452850542926058, -1.934965279058294518 ) ) ;
#6494 = CARTESIAN_POINT ( 'NONE',  ( -0.09506052544071567911, -63.49547149457075079, 6.999999999999997335 ) ) ;
#6495 = AXIS2_PLACEMENT_3D ( 'NONE', #92, #1403, #813 ) ;
#6496 = DIRECTION ( 'NONE',  ( 9.251858538542972814E-17, -1.000000000000000000, 0.000000000000000000 ) ) ;
#6497 = CARTESIAN_POINT ( 'NONE',  ( -4.725907263620320542, -78.90452850542925489, 1.635492904037698647 ) ) ;
#6498 = CARTESIAN_POINT ( 'NONE',  ( 7.360235569667880284, -88.24547149457073658, 0.09995255151716216091 ) ) ;
#6499 = DIRECTION ( 'NONE',  ( 0.000000000000000000, 0.000000000000000000, 1.000000000000000000 ) ) ;
#6500 = DIRECTION ( 'NONE',  ( 1.000000000000000000, 2.775557561562892337E-16, -0.000000000000000000 ) ) ;
#6501 = CARTESIAN_POINT ( 'NONE',  ( 3.015831842038231958, -58.80452850542925347, 3.989209796945429432 ) ) ;
#6502 = SHAPE_REPRESENTATION ( 'jaw base', ( #2840 ), #7820 ) ;
#6503 = CARTESIAN_POINT ( 'NONE',  ( -2.369498399071054529, -93.34547149457073090, 6.969112962950058332 ) ) ;
#6504 = ORIENTED_EDGE ( 'NONE', *, *, #5326, .F. ) ;
#6505 = CARTESIAN_POINT ( 'NONE',  ( 1.719659006605390283, -73.65452850542924068, 4.969112962950016588 ) ) ;
#6506 = CIRCLE ( 'NONE', #4348, 1.500000000000000666 ) ;
#6507 = PLANE ( 'NONE',  #5156 ) ;
#6508 = EDGE_CURVE ( 'NONE', #4681, #2858, #3315, .T. ) ;
#6509 = CIRCLE ( 'NONE', #2343, 5.000000000000004441 ) ;
#6510 = VECTOR ( 'NONE', #2263, 1000.000000000000000 ) ;
#6511 = DIRECTION ( 'NONE',  ( -9.251858538542971828E-16, 1.000000000000000000, 0.000000000000000000 ) ) ;
#6512 = CARTESIAN_POINT ( 'NONE',  ( -0.09506052544073428923, -84.49547149457075079, 4.999999999999997335 ) ) ;
#6513 = CARTESIAN_POINT ( 'NONE',  ( 6.123233995736760366E-16, -27.00000000000000000, -2.499999999999999556 ) ) ;
#6514 = CARTESIAN_POINT ( 'NONE',  ( -2.882544866740859746, -59.89547149457074937, 0.8366430509619596778 ) ) ;
#6515 = CARTESIAN_POINT ( 'NONE',  ( 6.628020296210639373, -65.40452850542925489, -2.253526892787612645 ) ) ;
#6516 = DIRECTION ( 'NONE',  ( 1.000000000000000000, 0.000000000000000000, 0.000000000000000000 ) ) ;
#6517 = CARTESIAN_POINT ( 'NONE',  ( 2.862020680886599333, -75.79547149457074795, 4.100960146803977580 ) ) ;
#6518 = CARTESIAN_POINT ( 'NONE',  ( -0.09506052544084261924, -57.00452850542924921, -4.999999999999997335 ) ) ;
#6519 = CARTESIAN_POINT ( 'NONE',  ( 1.529537955723691889, -86.85452850542921510, -5.030887037049978971 ) ) ;
#6520 = CARTESIAN_POINT ( 'NONE',  ( -5.895805022753386915, -64.05452850542924637, 4.407101234057909878 ) ) ;
#6521 = CIRCLE ( 'NONE', #7600, 6.000000000000000000 ) ;
#6522 = CARTESIAN_POINT ( 'NONE',  ( -2.493201789345291353, -74.44547149457072521, -1.934965279058240561 ) ) ;
#6523 = EDGE_CURVE ( 'NONE', #238, #6651, #3272, .T. ) ;
#6524 = VERTEX_POINT ( 'NONE', #7654 ) ;
#6525 = DIRECTION ( 'NONE',  ( 1.261617073437677752E-16, -1.000000000000000000, -0.000000000000000000 ) ) ;
#6526 = DIRECTION ( 'NONE',  ( 0.000000000000000000, 0.000000000000000000, -1.000000000000000000 ) ) ;
#6527 = CARTESIAN_POINT ( 'NONE',  ( -4.194503406049315153, -88.05452850542921794, 3.171033256558100533 ) ) ;
#6528 = ORIENTED_EDGE ( 'NONE', *, *, #3253, .F. ) ;
#6529 = CARTESIAN_POINT ( 'NONE',  ( 3.015831842038234623, -82.80452850542926058, 3.989209796945429432 ) ) ;
#6530 = CARTESIAN_POINT ( 'NONE',  ( 2.823794231030062107, -94.09547149457074511, 1.017458915287723809 ) ) ;
#6531 = DIRECTION ( 'NONE',  ( 0.000000000000000000, 0.000000000000000000, 1.000000000000000000 ) ) ;
#6532 = CARTESIAN_POINT ( 'NONE',  ( -4.312004677471056091, -87.45452850542925205, -3.009306630940844052 ) ) ;
#6533 = CARTESIAN_POINT ( 'NONE',  ( -0.09506052544085875911, -96.00452850542926342, -6.999999999999997335 ) ) ;
#6534 = CARTESIAN_POINT ( 'NONE',  ( -0.09506052544082008171, -69.00452850542926342, -2.999999999999997780 ) ) ;
#6535 = CARTESIAN_POINT ( 'NONE',  ( 50.00000000000000000, -9.999999999999994671, 10.50000000000000533 ) ) ;
#6536 = CARTESIAN_POINT ( 'NONE',  ( 80.00000000000000000, 0.000000000000000000, -20.00000000000000000 ) ) ;
#6537 = CARTESIAN_POINT ( 'NONE',  ( 2.882544866740897049, -80.10452850542927195, 0.8366430509618999478 ) ) ;
#6538 = CARTESIAN_POINT ( 'NONE',  ( -6.628020296210618056, -93.90452850542926910, 2.253526892787613978 ) ) ;
#6539 = CARTESIAN_POINT ( 'NONE',  ( -5.999999999999993783, -51.00000000000000711, -2.499999999999999112 ) ) ;
#6540 = CARTESIAN_POINT ( 'NONE',  ( 4.194503406049337357, -74.55452850542923215, -3.171033256558100089 ) ) ;
#6541 = CARTESIAN_POINT ( 'NONE',  ( 7.360235569667880284, -91.24547149457073658, 0.09995255151716216091 ) ) ;
#6542 = DIRECTION ( 'NONE',  ( -1.000000000000000000, -1.261617073437677752E-16, 0.000000000000000000 ) ) ;
#6543 = DIRECTION ( 'NONE',  ( 1.000000000000000000, 2.775557561562892337E-16, 0.000000000000000000 ) ) ;
#6544 = CARTESIAN_POINT ( 'NONE',  ( -3.154386672714791118, -68.74547149457075079, -0.09995255151720625064 ) ) ;
#6545 = CARTESIAN_POINT ( 'NONE',  ( -0.09506052544084224454, -60.00452850542925631, -4.999999999999997335 ) ) ;
#6546 = EDGE_LOOP ( 'NONE', ( #3579, #3829, #954, #5327 ) ) ;
#6547 = CARTESIAN_POINT ( 'NONE',  ( -4.191402346623055664, -90.19547149457073942, 5.607243785695398941 ) ) ;
#6548 = ORIENTED_EDGE ( 'NONE', *, *, #694, .F. ) ;
#6549 = CARTESIAN_POINT ( 'NONE',  ( -4.784657899331190123, -75.60452850542925773, -1.454677039711773867 ) ) ;
#6550 = CARTESIAN_POINT ( 'NONE',  ( 6.000000000000006217, -51.00000000000000711, -2.500000000000001776 ) ) ;
#6551 = DIRECTION ( 'NONE',  ( 1.000000000000000000, 0.000000000000000000, 0.000000000000000000 ) ) ;
#6552 = CARTESIAN_POINT ( 'NONE',  ( 1.529537955723796028, -84.64547149457074227, 5.030887037049945221 ) ) ;
#6553 = CARTESIAN_POINT ( 'NONE',  ( 4.230555499402125719, -97.00000000000000000, 2.192008249831833400 ) ) ;
#6554 = CARTESIAN_POINT ( 'NONE',  ( 2.610703060766943029, -64.54547149457073374, -1.773238653441125523 ) ) ;
#6555 = CARTESIAN_POINT ( 'NONE',  ( 6.628020296210639373, -68.40452850542925489, -2.253526892787612645 ) ) ;
#6556 = DIRECTION ( 'NONE',  ( 0.000000000000000000, -0.000000000000000000, -1.000000000000000000 ) ) ;
#6557 = CARTESIAN_POINT ( 'NONE',  ( -4.312004677470993030, -75.04547149457074795, 3.009306630940933758 ) ) ;
#6558 = DIRECTION ( 'NONE',  ( -1.000000000000000000, 8.326672684688674053E-16, 0.000000000000000000 ) ) ;
#6559 = CARTESIAN_POINT ( 'NONE',  ( 5.257311121191342806, -86.25452850542924921, -0.09995255151729465215 ) ) ;
#6560 = CARTESIAN_POINT ( 'NONE',  ( -5.895805022753386915, -70.05452850542926058, 4.407101234057909878 ) ) ;
#6561 = EDGE_CURVE ( 'NONE', #1092, #2153, #6509, .T. ) ;
#6562 = CARTESIAN_POINT ( 'NONE',  ( -0.8796985632579428227, -77.14547149457074227, -3.030887037049952326 ) ) ;
#6563 = AXIS2_PLACEMENT_3D ( 'NONE', #2717, #5192, #6542 ) ;
#6564 = VERTEX_POINT ( 'NONE', #101 ) ;
#6565 = DIRECTION ( 'NONE',  ( 0.000000000000000000, 2.168404344971010594E-16, -1.000000000000000000 ) ) ;
#6566 = CARTESIAN_POINT ( 'NONE',  ( -47.50000000000000711, -198.2344135219424857, 12.49999999999993960 ) ) ;
#6567 = CARTESIAN_POINT ( 'NONE',  ( -4.784657899331189235, -90.60452850542925773, -1.454677039711773867 ) ) ;
#6568 = EDGE_LOOP ( 'NONE', ( #6753, #4126 ) ) ;
#6569 = CARTESIAN_POINT ( 'NONE',  ( 1.529537955723690335, -77.85452850542924352, -5.030887037049978971 ) ) ;
#6570 = CARTESIAN_POINT ( 'NONE',  ( 1.686450176301637960, -90.79547149457074795, 2.482926158054096000 ) ) ;
#6571 =( LENGTH_UNIT ( ) NAMED_UNIT ( * ) SI_UNIT ( .MILLI., .METRE. ) );
#6572 = CARTESIAN_POINT ( 'NONE',  ( 2.862020680886515844, -89.70452850542926626, -4.100960146804039752 ) ) ;
#6573 = CARTESIAN_POINT ( 'NONE',  ( -5.895805022753383362, -94.05452850542926058, 4.407101234057909878 ) ) ;
#6574 = CARTESIAN_POINT ( 'NONE',  ( -2.610703060766966566, -63.45452850542924494, -1.773238653441072232 ) ) ;
#6575 = CARTESIAN_POINT ( 'NONE',  ( -1.499999999999999556, -9.999999999999994671, 0.000000000000000000 ) ) ;
#6576 = DIRECTION ( 'NONE',  ( -0.000000000000000000, -0.000000000000000000, -1.000000000000000000 ) ) ;
#6577 = CARTESIAN_POINT ( 'NONE',  ( -1.840261337453251489, -78.30452850542926058, -2.371175808195547852 ) ) ;
#6578 = CARTESIAN_POINT ( 'NONE',  ( 2.369498399071226835, -88.65452850542926910, 6.969112962950009482 ) ) ;
#6579 = AXIS2_PLACEMENT_3D ( 'NONE', #5436, #3580, #4048 ) ;
#6580 = CARTESIAN_POINT ( 'NONE',  ( -80.00000000000000000, 0.000000000000000000, 20.00000000000000000 ) ) ;
#6581 = CARTESIAN_POINT ( 'NONE',  ( -4.191402346623057440, -84.19547149457073942, 5.607243785695398941 ) ) ;
#6582 = LINE ( 'NONE', #812, #774 ) ;
#6583 = CARTESIAN_POINT ( 'NONE',  ( 50.00000000000000000, 1.734723475976807094E-15, -12.50000000000000000 ) ) ;
#6584 = CARTESIAN_POINT ( 'NONE',  ( -2.882544866740858414, -68.89547149457074227, 0.8366430509619596778 ) ) ;
#6585 = AXIS2_PLACEMENT_3D ( 'NONE', #2616, #5851, #79 ) ;
#6586 = ADVANCED_FACE ( 'NONE', ( #5200 ), #3816, .T. ) ;
#6587 = AXIS2_PLACEMENT_3D ( 'NONE', #6330, #3041, #5015 ) ;
#6588 = ORIENTED_EDGE ( 'NONE', *, *, #1659, .F. ) ;
#6589 = CARTESIAN_POINT ( 'NONE',  ( -3.015831842038215971, -69.30452850542926058, -3.989209796945429432 ) ) ;
#6590 = CARTESIAN_POINT ( 'NONE',  ( -0.09506052544071304233, -84.49547149457075079, 6.999999999999997335 ) ) ;
#6591 = ORIENTED_EDGE ( 'NONE', *, *, #1981, .T. ) ;
#6592 = CIRCLE ( 'NONE', #4701, 1.499999999999999556 ) ;
#6593 = CARTESIAN_POINT ( 'NONE',  ( 4.784657899331208775, -71.10452850542925773, 1.454677039711774533 ) ) ;
#6594 = CARTESIAN_POINT ( 'NONE',  ( -80.00000000000000000, -2.168404344971008868E-15, 12.50000000000000000 ) ) ;
#6595 = ADVANCED_FACE ( 'NONE', ( #6348 ), #3939, .F. ) ;
#6596 = CARTESIAN_POINT ( 'NONE',  ( -1.719659006605267049, -66.34547149457073090, 4.969112962950051227 ) ) ;
#6597 = CYLINDRICAL_SURFACE ( 'NONE', #3634, 1.500000000000001776 ) ;
#6598 = CARTESIAN_POINT ( 'NONE',  ( 4.194503406049402194, -96.94547149457073942, 3.171033256558012159 ) ) ;
#6599 = CARTESIAN_POINT ( 'NONE',  ( 4.037591185471441690, -68.70452850542925205, -5.718994135553947977 ) ) ;
#6600 = DIRECTION ( 'NONE',  ( 1.000000000000000000, 0.000000000000000000, 0.000000000000000000 ) ) ;
#6601 = CARTESIAN_POINT ( 'NONE',  ( -4.194503406049315153, -88.05452850542921794, 3.171033256558100533 ) ) ;
#6602 =( GEOMETRIC_REPRESENTATION_CONTEXT ( 3 ) GLOBAL_UNCERTAINTY_ASSIGNED_CONTEXT ( ( #1656 ) ) GLOBAL_UNIT_ASSIGNED_CONTEXT ( ( #4224, #509, #1621 ) ) REPRESENTATION_CONTEXT ( 'NONE', 'WORKASPACE' ) );
#6603 = CARTESIAN_POINT ( 'NONE',  ( 7.360235569667877620, -65.25452850542926342, -0.09995255151731691212 ) ) ;
#6604 = CARTESIAN_POINT ( 'NONE',  ( 1.686450176301636850, -81.79547149457074795, 2.482926158054096000 ) ) ;
#6605 = ORIENTED_EDGE ( 'NONE', *, *, #2976, .T. ) ;
#6606 = DIRECTION ( 'NONE',  ( -0.000000000000000000, -0.000000000000000000, -1.000000000000000000 ) ) ;
#6607 = CARTESIAN_POINT ( 'NONE',  ( 4.725907263620342746, -95.40452850542925489, -1.635492904037697981 ) ) ;
#6608 = CARTESIAN_POINT ( 'NONE',  ( -4.784657899331189235, -87.60452850542925773, -1.454677039711773867 ) ) ;
#6609 = ORIENTED_EDGE ( 'NONE', *, *, #7691, .F. ) ;
#6610 = CARTESIAN_POINT ( 'NONE',  ( -4.725907263620321430, -72.90452850542925489, 1.635492904037698647 ) ) ;
#6611 = CARTESIAN_POINT ( 'NONE',  ( -0.8796985632579410463, -92.14547149457074227, -3.030887037049952326 ) ) ;
#6612 = ADVANCED_FACE ( 'NONE', ( #6388 ), #4438, .F. ) ;
#6613 = CARTESIAN_POINT ( 'NONE',  ( -1.529537955723668796, -85.35452850542924352, 5.030887037049979860 ) ) ;
#6614 = CARTESIAN_POINT ( 'NONE',  ( 5.895805022753492608, -63.94547149457074653, 4.407101234057782868 ) ) ;
#6615 = CARTESIAN_POINT ( 'NONE',  ( 1.069819614139555730, -64.65452850542924068, 2.969112962950023249 ) ) ;
#6616 = ADVANCED_FACE ( 'NONE', ( #566, #5742 ), #4395, .F. ) ;
#6617 = DIRECTION ( 'NONE',  ( 1.000000000000000000, 0.000000000000000000, 0.000000000000000000 ) ) ;
#6618 = DIRECTION ( 'NONE',  ( -0.000000000000000000, -1.000000000000000000, -0.000000000000000000 ) ) ;
#6619 = CARTESIAN_POINT ( 'NONE',  ( 2.610703060766983885, -76.95452850542926626, 1.773238653441072232 ) ) ;
#6620 = CARTESIAN_POINT ( 'NONE',  ( 0.09506052544088325340, -91.50452850542926342, 6.999999999999997335 ) ) ;
#6621 = CARTESIAN_POINT ( 'NONE',  ( -7.360235569667858080, -86.74547149457075079, -0.09995255151716124498 ) ) ;
#6622 = FACE_OUTER_BOUND ( 'NONE', #1040, .T. ) ;
#6623 = CARTESIAN_POINT ( 'NONE',  ( 55.00000000000002132, -88.00000000000000000, 0.000000000000000000 ) ) ;
#6624 = CARTESIAN_POINT ( 'NONE',  ( 1.840261337453218848, -64.69547149457073942, -2.371175808195584267 ) ) ;
#6625 = EDGE_LOOP ( 'NONE', ( #6038, #7688, #1116, #482 ) ) ;
#6626 = AXIS2_PLACEMENT_3D ( 'NONE', #7300, #6500, #5233 ) ;
#6627 = CARTESIAN_POINT ( 'NONE',  ( -4.725907263620322318, -69.90452850542925489, 1.635492904037698647 ) ) ;
#6628 = CARTESIAN_POINT ( 'NONE',  ( -5.895805022753477509, -77.44547149457073942, -4.407101234057782868 ) ) ;
#6629 = VERTEX_POINT ( 'NONE', #5117 ) ;
#6630 = CARTESIAN_POINT ( 'NONE',  ( -4.725907263620323207, -60.90452850542925489, 1.635492904037698647 ) ) ;
#6631 = DIRECTION ( 'NONE',  ( 0.000000000000000000, -1.000000000000000000, 0.000000000000000000 ) ) ;
#6632 = APPLICATION_CONTEXT ( 'automotive_design' ) ;
#6633 = CONTEXT_DEPENDENT_SHAPE_REPRESENTATION ( #396, #1039 ) ;
#6634 = CARTESIAN_POINT ( 'NONE',  ( -0.09506052544073578803, -72.49547149457075079, 4.999999999999997335 ) ) ;
#6635 = CARTESIAN_POINT ( 'NONE',  ( 3.943604702053941724E-15, -22.00000000000000000, 0.000000000000000000 ) ) ;
#6636 = CARTESIAN_POINT ( 'NONE',  ( -2.493201789345292241, -65.44547149457075363, -1.934965279058240561 ) ) ;
#6637 = CARTESIAN_POINT ( 'NONE',  ( 4.191402346623195996, -64.80452850542926058, 5.607243785695311900 ) ) ;
#6638 = PLANE ( 'NONE',  #7386 ) ;
#6639 = AXIS2_PLACEMENT_3D ( 'NONE', #3104, #6304, #7529 ) ;
#6640 = EDGE_CURVE ( 'NONE', #5386, #1922, #3685, .T. ) ;
#6641 = SURFACE_SIDE_STYLE ('',( #1503 ) ) ;
#6642 = CARTESIAN_POINT ( 'NONE',  ( -5.257311121191323267, -81.75452850542926342, 0.09995255151729526277 ) ) ;
#6643 = CARTESIAN_POINT ( 'NONE',  ( 6.013306294175167821, -61.95452850542925916, 4.245374608440616093 ) ) ;
#6644 = CARTESIAN_POINT ( 'NONE',  ( -0.8796985632579424896, -80.14547149457074227, -3.030887037049952326 ) ) ;
#6645 = CIRCLE ( 'NONE', #1538, 1.500000000000000666 ) ;
#6646 = EDGE_CURVE ( 'NONE', #1594, #3416, #5701, .T. ) ;
#6647 = ORIENTED_EDGE ( 'NONE', *, *, #4088, .F. ) ;
#6648 = FACE_OUTER_BOUND ( 'NONE', #2999, .T. ) ;
#6649 = CARTESIAN_POINT ( 'NONE',  ( 80.00000000000000000, -7.999999999999992895, -12.50000000000000178 ) ) ;
#6650 = CARTESIAN_POINT ( 'NONE',  ( -3.015831842038214639, -78.30452850542926058, -3.989209796945429432 ) ) ;
#6651 = VERTEX_POINT ( 'NONE', #1245 ) ;
#6652 = CARTESIAN_POINT ( 'NONE',  ( -4.312004677471057867, -75.45452850542926626, -3.009306630940843608 ) ) ;
#6653 = CARTESIAN_POINT ( 'NONE',  ( 0.09506052544077779609, -88.99547149457075079, -2.999999999999997780 ) ) ;
#6654 = AXIS2_PLACEMENT_3D ( 'NONE', #2850, #7991, #3938 ) ;
#6655 = CARTESIAN_POINT ( 'NONE',  ( 4.194503406049402194, -96.94547149457073942, 3.171033256558012159 ) ) ;
#6656 = CARTESIAN_POINT ( 'NONE',  ( -4.191402346623060104, -63.19547149457074653, 5.607243785695398941 ) ) ;
#6657 = CARTESIAN_POINT ( 'NONE',  ( 0.09506052544083806732, -70.50452850542926342, 2.999999999999997780 ) ) ;
#6658 = VERTEX_POINT ( 'NONE', #7694 ) ;
#6659 = CARTESIAN_POINT ( 'NONE',  ( 50.00000000000000000, 1.734723475976807094E-15, -12.50000000000000000 ) ) ;
#6660 = FACE_BOUND ( 'NONE', #6026, .T. ) ;
#6661 = CARTESIAN_POINT ( 'NONE',  ( 2.823794231030040791, -77.40452850542925489, -1.017458915287783316 ) ) ;
#6662 = CARTESIAN_POINT ( 'NONE',  ( -6.686770931921503625, -93.60452850542925773, -2.072711028461647675 ) ) ;
#6663 = CARTESIAN_POINT ( 'NONE',  ( 2.179377348189631025, -90.64547149457075648, 7.030887037049939003 ) ) ;
#6664 = CARTESIAN_POINT ( 'NONE',  ( -80.00000000000000000, -25.00000000000000000, -20.00000000000000000 ) ) ;
#6665 = DIRECTION ( 'NONE',  ( 1.000000000000000000, -0.000000000000000000, -0.000000000000000000 ) ) ;
#6666 = CARTESIAN_POINT ( 'NONE',  ( 1.069819614139493114, -67.84547149457071669, -2.969112962950042789 ) ) ;
#6667 = DIRECTION ( 'NONE',  ( 1.000000000000000000, 0.000000000000000000, 0.000000000000000000 ) ) ;
#6668 = ORIENTED_EDGE ( 'NONE', *, *, #5697, .F. ) ;
#6669 = CARTESIAN_POINT ( 'NONE',  ( 4.194503406049335581, -65.55452850542923215, -3.171033256558100089 ) ) ;
#6670 = CARTESIAN_POINT ( 'NONE',  ( 5.895805022753496161, -75.94547149457073942, 4.407101234057782868 ) ) ;
#6671 =( NAMED_UNIT ( * ) SI_UNIT ( $, .STERADIAN. ) SOLID_ANGLE_UNIT ( ) );
#6672 = VERTEX_POINT ( 'NONE', #4479 ) ;
#6673 = CARTESIAN_POINT ( 'NONE',  ( -5.257311121191324155, -69.75452850542926342, 0.09995255151729526277 ) ) ;
#6674 = DIRECTION ( 'NONE',  ( 0.000000000000000000, 0.000000000000000000, 1.000000000000000000 ) ) ;
#6675 = ADVANCED_FACE ( 'NONE', ( #7059 ), #644, .T. ) ;
#6676 = CARTESIAN_POINT ( 'NONE',  ( 0.09506052544075450916, -70.99547149457075079, -4.999999999999997335 ) ) ;
#6677 = CARTESIAN_POINT ( 'NONE',  ( 80.00000000000000000, -12.00000000000000711, 12.49999999999999822 ) ) ;
#6678 = CARTESIAN_POINT ( 'NONE',  ( -2.862020680886578461, -95.29547149457074795, -4.100960146803977580 ) ) ;
#6679 = CARTESIAN_POINT ( 'NONE',  ( 2.369498399071223727, -64.65452850542924068, 6.969112962950009482 ) ) ;
#6680 = ORIENTED_EDGE ( 'NONE', *, *, #8250, .F. ) ;
#6681 = SURFACE_STYLE_FILL_AREA ( #4697 ) ;
#6682 = CARTESIAN_POINT ( 'NONE',  ( 3.015831842038235067, -85.80452850542926058, 3.989209796945429432 ) ) ;
#6683 = EDGE_LOOP ( 'NONE', ( #5468, #4938, #5619 ) ) ;
#6684 = DIRECTION ( 'NONE',  ( 2.775557561562892337E-16, -1.000000000000000000, 0.000000000000000000 ) ) ;
#6685 = CARTESIAN_POINT ( 'NONE',  ( 4.194503406049339134, -86.55452850542926058, -3.171033256558100089 ) ) ;
#6686 = CARTESIAN_POINT ( 'NONE',  ( -2.862020680886494528, -76.20452850542926626, 4.100960146804039752 ) ) ;
#6687 = ORIENTED_EDGE ( 'NONE', *, *, #8014, .F. ) ;
#6688 = CARTESIAN_POINT ( 'NONE',  ( 4.784657899331208775, -71.10452850542925773, 1.454677039711774533 ) ) ;
#6689 = CARTESIAN_POINT ( 'NONE',  ( 1.686450176301637516, -87.79547149457074795, 2.482926158054096000 ) ) ;
#6690 = CARTESIAN_POINT ( 'NONE',  ( -1.069819614139476460, -63.34547149457073800, 2.969112962950044121 ) ) ;
#6691 = CARTESIAN_POINT ( 'NONE',  ( 1.529537955723690112, -77.85452850542922931, -5.030887037049978971 ) ) ;
#6692 = CARTESIAN_POINT ( 'NONE',  ( -0.09506052544085952238, -90.00452850542926342, -6.999999999999997335 ) ) ;
#6693 = VECTOR ( 'NONE', #257, 1000.000000000000000 ) ;
#6694 = CARTESIAN_POINT ( 'NONE',  ( -2.882544866740879286, -60.60452850542926484, -0.8366430509618996147 ) ) ;
#6695 = EDGE_LOOP ( 'NONE', ( #3376, #3606, #2283 ) ) ;
#6696 = CARTESIAN_POINT ( 'NONE',  ( -80.00000000000000000, 0.000000000000000000, 20.00000000000000000 ) ) ;
#6697 = DIRECTION ( 'NONE',  ( -1.000000000000000000, 0.000000000000000000, 0.000000000000000000 ) ) ;
#6698 = CARTESIAN_POINT ( 'NONE',  ( -2.882544866740877509, -75.60452850542924352, -0.8366430509618996147 ) ) ;
#6699 = CARTESIAN_POINT ( 'NONE',  ( -4.191402346623177344, -87.30452850542926058, -5.607243785695311900 ) ) ;
#6700 = CARTESIAN_POINT ( 'NONE',  ( -4.037591185471544719, -80.29547149457074795, -5.718994135553860936 ) ) ;
#6701 = CARTESIAN_POINT ( 'NONE',  ( 45.19324698792023298, -11.84363253063589205, 4.500000000000000888 ) ) ;
#6702 = CARTESIAN_POINT ( 'NONE',  ( -0.7729879516809968765, -24.10129518119626013, 2.500000000000000888 ) ) ;
#6703 = CARTESIAN_POINT ( 'NONE',  ( 1.686450176301634185, -63.79547149457074084, 2.482926158054096000 ) ) ;
#6704 = PRODUCT_DEFINITION_CONTEXT ( 'detailed design', #7181, 'design' ) ;
#6705 = PLANE ( 'NONE',  #2472 ) ;
#6706 = ORIENTED_EDGE ( 'NONE', *, *, #4992, .T. ) ;
#6707 = EDGE_CURVE ( 'NONE', #8040, #4798, #14, .T. ) ;
#6708 = CARTESIAN_POINT ( 'NONE',  ( 54.99999999999999289, -9.999999999999994671, 0.000000000000000000 ) ) ;
#6709 = CARTESIAN_POINT ( 'NONE',  ( 1.719659006605389173, -64.65452850542925489, 4.969112962950016588 ) ) ;
#6710 = CIRCLE ( 'NONE', #4688, 3.000000000000002665 ) ;
#6711 = CARTESIAN_POINT ( 'NONE',  ( -4.191402346623057440, -84.19547149457073942, 5.607243785695398941 ) ) ;
#6712 =( NAMED_UNIT ( * ) SI_UNIT ( $, .STERADIAN. ) SOLID_ANGLE_UNIT ( ) );
#6713 = EDGE_LOOP ( 'NONE', ( #8200, #4235, #3438, #6730 ) ) ;
#6714 = CARTESIAN_POINT ( 'NONE',  ( 5.257311121191341030, -76.24547149457073658, 0.09995255151718437925 ) ) ;
#6715 = CARTESIAN_POINT ( 'NONE',  ( 0.09506052544075488386, -73.99547149457075079, -4.999999999999997335 ) ) ;
#6716 = CARTESIAN_POINT ( 'NONE',  ( -2.862020680886495416, -70.20452850542925205, 4.100960146804039752 ) ) ;
#6717 = DIRECTION ( 'NONE',  ( 0.000000000000000000, 0.000000000000000000, -1.000000000000000000 ) ) ;
#6718 = VECTOR ( 'NONE', #7214, 1000.000000000000000 ) ;
#6719 = DIRECTION ( 'NONE',  ( 0.000000000000000000, 0.000000000000000000, -1.000000000000000000 ) ) ;
#6720 = CARTESIAN_POINT ( 'NONE',  ( -4.194503406049384431, -74.44547149457071100, -3.171033256558012159 ) ) ;
#6721 = FACE_OUTER_BOUND ( 'NONE', #2175, .T. ) ;
#6722 = CARTESIAN_POINT ( 'NONE',  ( 0.09506052544087986722, -64.50452850542926342, 6.999999999999997335 ) ) ;
#6723 = ORIENTED_EDGE ( 'NONE', *, *, #5676, .F. ) ;
#6724 = FILL_AREA_STYLE_COLOUR ( '', #5884 ) ;
#6725 = VECTOR ( 'NONE', #3387, 1000.000000000000000 ) ;
#6726 = ORIENTED_EDGE ( 'NONE', *, *, #2592, .F. ) ;
#6727 = PLANE ( 'NONE',  #1938 ) ;
#6728 = CARTESIAN_POINT ( 'NONE',  ( 5.257311121191342806, -86.25452850542924921, -0.09995255151729465215 ) ) ;
#6729 = CARTESIAN_POINT ( 'NONE',  ( -4.194503406049316041, -79.05452850542921794, 3.171033256558100533 ) ) ;
#6730 = ORIENTED_EDGE ( 'NONE', *, *, #3356, .T. ) ;
#6731 = CARTESIAN_POINT ( 'NONE',  ( -4.784657899331190123, -75.60452850542925773, -1.454677039711773867 ) ) ;
#6732 = CARTESIAN_POINT ( 'NONE',  ( 2.493201789345310893, -84.94547149457073942, 1.934965279058241006 ) ) ;
#6733 = PRESENTATION_LAYER_ASSIGNMENT (  '', '', ( #5919 ) ) ;
#6734 = CARTESIAN_POINT ( 'NONE',  ( 0.09506052544077440991, -61.99547149457073658, -2.999999999999997780 ) ) ;
#6735 = CARTESIAN_POINT ( 'NONE',  ( 4.784657899331209663, -77.10452850542925773, 1.454677039711774533 ) ) ;
#6736 = CARTESIAN_POINT ( 'NONE',  ( 5.895805022753407343, -86.55452850542926058, -4.407101234057908989 ) ) ;
#6737 = CARTESIAN_POINT ( 'NONE',  ( -2.493201789345254049, -61.05452850542925347, 1.934965279058294518 ) ) ;
#6738 = ORIENTED_EDGE ( 'NONE', *, *, #694, .T. ) ;
#6739 = DIRECTION ( 'NONE',  ( 1.000000000000000000, 2.775557561562892337E-16, -0.000000000000000000 ) ) ;
#6740 = ORIENTED_EDGE ( 'NONE', *, *, #2370, .F. ) ;
#6741 = DIRECTION ( 'NONE',  ( 0.000000000000000000, 0.000000000000000000, -1.000000000000000000 ) ) ;
#6742 = CARTESIAN_POINT ( 'NONE',  ( 3.154386672714807105, -65.25452850542926342, -0.09995255151727241993 ) ) ;
#6743 = CARTESIAN_POINT ( 'NONE',  ( -5.895805022753386027, -79.05452850542926058, 4.407101234057909878 ) ) ;
#6744 = CARTESIAN_POINT ( 'NONE',  ( 5.895805022753496161, -81.94547149457073942, 4.407101234057782868 ) ) ;
#6745 = DIRECTION ( 'NONE',  ( -0.000000000000000000, 0.000000000000000000, 1.000000000000000000 ) ) ;
#6746 = EDGE_CURVE ( 'NONE', #4058, #250, #4520, .T. ) ;
#6747 = DIRECTION ( 'NONE',  ( 0.000000000000000000, -1.000000000000000000, 0.000000000000000000 ) ) ;
#6748 = CARTESIAN_POINT ( 'NONE',  ( -0.8796985632578782077, -85.35452850542924352, 3.030887037049973198 ) ) ;
#6749 = ORIENTED_EDGE ( 'NONE', *, *, #576, .T. ) ;
#6750 = LINE ( 'NONE', #7190, #6379 ) ;
#6751 = CARTESIAN_POINT ( 'NONE',  ( 5.257311121191341918, -68.25452850542926342, -0.09995255151729465215 ) ) ;
#6752 = CARTESIAN_POINT ( 'NONE',  ( 0.09506052544073424759, -76.99547149457075079, -6.999999999999997335 ) ) ;
#6753 = ORIENTED_EDGE ( 'NONE', *, *, #6134, .F. ) ;
#6754 = PRODUCT_DEFINITION_SHAPE ( 'NONE', 'NONE',  #8338 ) ;
#6755 = CARTESIAN_POINT ( 'NONE',  ( -2.862020680886580681, -77.29547149457074795, -4.100960146803977580 ) ) ;
#6756 = CARTESIAN_POINT ( 'NONE',  ( 1.719659006605284590, -67.84547149457070248, -4.969112962950050338 ) ) ;
#6757 = CARTESIAN_POINT ( 'NONE',  ( 4.312004677471073855, -64.95452850542926626, 3.009306630940844496 ) ) ;
#6758 = CARTESIAN_POINT ( 'NONE',  ( 80.00000000000000000, -9.999999999999994671, -1.500000000000000666 ) ) ;
#6759 = ADVANCED_FACE ( 'NONE', ( #8068 ), #4140, .F. ) ;
#6760 = CARTESIAN_POINT ( 'NONE',  ( 4.784657899331176800, -70.39547149457074227, -1.454677039711874009 ) ) ;
#6761 = CARTESIAN_POINT ( 'NONE',  ( 6.013306294175167821, -64.95452850542926626, 4.245374608440616093 ) ) ;
#6762 = ORIENTED_EDGE ( 'NONE', *, *, #8112, .F. ) ;
#6763 = DIRECTION ( 'NONE',  ( 0.000000000000000000, -2.775557561562891351E-16, 1.000000000000000000 ) ) ;
#6764 = ORIENTED_EDGE ( 'NONE', *, *, #777, .F. ) ;
#6765 = DIRECTION ( 'NONE',  ( -0.000000000000000000, -0.000000000000000000, -1.000000000000000000 ) ) ;
#6766 = CARTESIAN_POINT ( 'NONE',  ( 4.725907263620340970, -83.40452850542925489, -1.635492904037697981 ) ) ;
#6767 = CARTESIAN_POINT ( 'NONE',  ( -1.529537955723670128, -79.35452850542925773, 5.030887037049979860 ) ) ;
#6768 = ORIENTED_EDGE ( 'NONE', *, *, #43, .T. ) ;
#6769 = CARTESIAN_POINT ( 'NONE',  ( -1.529537955723670350, -76.35452850542925773, 5.030887037049979860 ) ) ;
#6770 = CARTESIAN_POINT ( 'NONE',  ( 1.686450176301636183, -78.79547149457074795, 2.482926158054096000 ) ) ;
#6771 = CARTESIAN_POINT ( 'NONE',  ( 1.069819614139492447, -61.84547149457074511, -2.969112962950042789 ) ) ;
#6772 = CARTESIAN_POINT ( 'NONE',  ( 5.257311121191341918, -71.25452850542923500, -0.09995255151729465215 ) ) ;
#6773 = CARTESIAN_POINT ( 'NONE',  ( -2.369498399071205075, -90.15452850542926910, -6.969112962950009482 ) ) ;
#6774 = EDGE_CURVE ( 'NONE', #4647, #1658, #5286, .T. ) ;
#6775 = VECTOR ( 'NONE', #660, 1000.000000000000000 ) ;
#6776 = VECTOR ( 'NONE', #4562, 1000.000000000000000 ) ;
#6777 = CARTESIAN_POINT ( 'NONE',  ( -1.840261337453198198, -93.19547149457075363, 2.371175808195584267 ) ) ;
#6778 = APPLICATION_PROTOCOL_DEFINITION ( 'draft international standard', 'automotive_design', 1998, #1421 ) ;
#6779 = VERTEX_POINT ( 'NONE', #1574 ) ;
#6780 = DIRECTION ( 'NONE',  ( 0.000000000000000000, 0.000000000000000000, -1.000000000000000000 ) ) ;
#6781 = VECTOR ( 'NONE', #4560, 1000.000000000000000 ) ;
#6782 = VERTEX_POINT ( 'NONE', #146 ) ;
#6783 = DIRECTION ( 'NONE',  ( 1.000000000000000000, 0.000000000000000000, 0.000000000000000000 ) ) ;
#6784 = CARTESIAN_POINT ( 'NONE',  ( -2.882544866740877954, -72.60452850542924352, -0.8366430509618996147 ) ) ;
#6785 = CARTESIAN_POINT ( 'NONE',  ( 0.09506052544073462229, -79.99547149457075079, -6.999999999999997335 ) ) ;
#6786 = DIRECTION ( 'NONE',  ( -0.000000000000000000, 3.469446951953615175E-16, 1.000000000000000000 ) ) ;
#6787 = CARTESIAN_POINT ( 'NONE',  ( -3.015831842038126709, -93.19547149457075363, 3.989209796945492048 ) ) ;
#6788 = CARTESIAN_POINT ( 'NONE',  ( 2.493201789345272701, -89.55452850542926058, -1.934965279058294518 ) ) ;
#6789 = VECTOR ( 'NONE', #3608, 1000.000000000000000 ) ;
#6790 = PRODUCT_DEFINITION_CONTEXT ( 'detailed design', #2603, 'design' ) ;
#6791 = CARTESIAN_POINT ( 'NONE',  ( -55.00000000000000000, -25.00000000000002132, 20.00000000000000000 ) ) ;
#6792 = ORIENTED_EDGE ( 'NONE', *, *, #3768, .F. ) ;
#6793 = LINE ( 'NONE', #2335, #862 ) ;
#6794 = CARTESIAN_POINT ( 'NONE',  ( -4.312004677471061420, -57.45452850542925916, -3.009306630940844052 ) ) ;
#6795 = CARTESIAN_POINT ( 'NONE',  ( -2.369498399071058969, -66.34547149457073090, 6.969112962950058332 ) ) ;
#6796 = CARTESIAN_POINT ( 'NONE',  ( 47.50000000000002132, -54.00000000000000711, 12.50000000000001954 ) ) ;
#6797 = CARTESIAN_POINT ( 'NONE',  ( 3.015831842038149357, -79.69547149457075363, -3.989209796945492048 ) ) ;
#6798 = CARTESIAN_POINT ( 'NONE',  ( 4.312004677471011682, -67.54547149457074795, -3.009306630940933314 ) ) ;
#6799 = CARTESIAN_POINT ( 'NONE',  ( -4.312004677471058756, -66.45452850542925205, -3.009306630940844052 ) ) ;
#6800 = CARTESIAN_POINT ( 'NONE',  ( -65.00000000000000000, -9.999999999999991118, -10.50000000000000888 ) ) ;
#6801 = CARTESIAN_POINT ( 'NONE',  ( 4.725907263620371168, -61.09547149457074511, 1.635492904037598283 ) ) ;
#6802 = PRESENTATION_STYLE_ASSIGNMENT (( #5656 ) ) ;
#6803 = CARTESIAN_POINT ( 'NONE',  ( 4.191402346623195996, -61.80452850542926058, 5.607243785695311900 ) ) ;
#6804 = ORIENTED_EDGE ( 'NONE', *, *, #726, .F. ) ;
#6805 = CARTESIAN_POINT ( 'NONE',  ( 54.99999999999999289, -9.999999999999994671, 1.500000000000000666 ) ) ;
#6806 = ORIENTED_EDGE ( 'NONE', *, *, #777, .T. ) ;
#6807 = LINE ( 'NONE', #7490, #8260 ) ;
#6808 = CARTESIAN_POINT ( 'NONE',  ( 3.015831842038234623, -82.80452850542926058, 3.989209796945429432 ) ) ;
#6809 = CARTESIAN_POINT ( 'NONE',  ( 3.015831842038233734, -73.80452850542926058, 3.989209796945429432 ) ) ;
#6810 = EDGE_CURVE ( 'NONE', #7328, #1819, #7826, .T. ) ;
#6811 = CARTESIAN_POINT ( 'NONE',  ( 4.725907263620339194, -62.40452850542925489, -1.635492904037697981 ) ) ;
#6812 = CARTESIAN_POINT ( 'NONE',  ( 2.610703060766945693, -76.54547149457074795, -1.773238653441125523 ) ) ;
#6813 = CARTESIAN_POINT ( 'NONE',  ( 5.257311121191342806, -94.24547149457070816, 0.09995255151718437925 ) ) ;
#6814 = EDGE_CURVE ( 'NONE', #1922, #5386, #5826, .T. ) ;
#6815 = CARTESIAN_POINT ( 'NONE',  ( -0.09506052544084073186, -72.00452850542926342, -4.999999999999997335 ) ) ;
#6816 = CARTESIAN_POINT ( 'NONE',  ( 6.013306294175171374, -91.95452850542925205, 4.245374608440616093 ) ) ;
#6817 = CARTESIAN_POINT ( 'NONE',  ( -1.686450176301614645, -95.29547149457076216, -2.482926158054096000 ) ) ;
#6818 = ORIENTED_EDGE ( 'NONE', *, *, #7587, .F. ) ;
#6819 = PLANE ( 'NONE',  #2014 ) ;
#6820 = ORIENTED_EDGE ( 'NONE', *, *, #2281, .F. ) ;
#6821 = CARTESIAN_POINT ( 'NONE',  ( 4.784657899331211439, -86.10452850542925773, 1.454677039711774533 ) ) ;
#6822 = CARTESIAN_POINT ( 'NONE',  ( 0.8796985632578985248, -71.85452850542924352, -3.030887037049972310 ) ) ;
#6823 = CARTESIAN_POINT ( 'NONE',  ( 2.179377348189629249, -75.64547149457072805, 7.030887037049939003 ) ) ;
#6824 = CARTESIAN_POINT ( 'NONE',  ( 2.862020680886516288, -92.70452850542926626, -4.100960146804039752 ) ) ;
#6825 = CARTESIAN_POINT ( 'NONE',  ( -1.529537955723774934, -92.14547149457074227, -5.030887037049945221 ) ) ;
#6826 = CARTESIAN_POINT ( 'NONE',  ( 1.686450176301586223, -83.70452850542925205, -2.482926158054133303 ) ) ;
#6827 = VECTOR ( 'NONE', #1612, 1000.000000000000000 ) ;
#6828 = VECTOR ( 'NONE', #3234, 1000.000000000000000 ) ;
#6829 = DIRECTION ( 'NONE',  ( -0.000000000000000000, -0.000000000000000000, -1.000000000000000000 ) ) ;
#6830 = ORIENTED_EDGE ( 'NONE', *, *, #5897, .T. ) ;
#6831 = DIRECTION ( 'NONE',  ( 0.000000000000000000, -1.000000000000000000, -1.734723475976807094E-16 ) ) ;
#6832 = CARTESIAN_POINT ( 'NONE',  ( -3.015831842038217303, -57.30452850542925347, -3.989209796945429432 ) ) ;
#6833 = CARTESIAN_POINT ( 'NONE',  ( -2.179377348189611485, -74.14547149457074227, -7.030887037049939003 ) ) ;
#6834 =( NAMED_UNIT ( * ) SI_UNIT ( $, .STERADIAN. ) SOLID_ANGLE_UNIT ( ) );
#6835 = CARTESIAN_POINT ( 'NONE',  ( 3.372186075517463966, -96.99999999999994316, -4.939745490940889994 ) ) ;
#6836 = CARTESIAN_POINT ( 'NONE',  ( 2.862020680886599333, -72.79547149457074795, 4.100960146803977580 ) ) ;
#6837 = CARTESIAN_POINT ( 'NONE',  ( -4.312004677470994807, -66.04547149457074795, 3.009306630940933758 ) ) ;
#6838 = CARTESIAN_POINT ( 'NONE',  ( -4.312004677471060532, -60.45452850542923784, -3.009306630940844052 ) ) ;
#6839 = CARTESIAN_POINT ( 'NONE',  ( -5.999999999999988454, -100.0010000000000048, -2.499999999999999112 ) ) ;
#6840 = EDGE_CURVE ( 'NONE', #3952, #5980, #2475, .T. ) ;
#6841 = CARTESIAN_POINT ( 'NONE',  ( -4.725907263620356069, -59.59547149457074511, -1.635492904037597617 ) ) ;
#6842 = CARTESIAN_POINT ( 'NONE',  ( -4.312004677471055203, -93.45452850542922363, -3.009306630940844052 ) ) ;
#6843 = VERTEX_POINT ( 'NONE', #344 ) ;
#6844 = VECTOR ( 'NONE', #91, 1000.000000000000000 ) ;
#6845 = AXIS2_PLACEMENT_3D ( 'NONE', #8137, #1857, #4250 ) ;
#6846 = CARTESIAN_POINT ( 'NONE',  ( 50.00000000000000000, -9.999999999999991118, -10.50000000000000888 ) ) ;
#6847 = PRODUCT_DEFINITION ( 'UNKNOWN', '', #6314, #7384 ) ;
#6848 = PRODUCT_DEFINITION_FORMATION_WITH_SPECIFIED_SOURCE ( 'ANY', '', #1788, .NOT_KNOWN. ) ;
#6849 = ORIENTED_EDGE ( 'NONE', *, *, #4850, .F. ) ;
#6850 = CARTESIAN_POINT ( 'NONE',  ( 50.00000000000000000, -19.99999999999999645, -12.50000000000000355 ) ) ;
#6851 = CARTESIAN_POINT ( 'NONE',  ( 4.784657899331211439, -86.10452850542925773, 1.454677039711774533 ) ) ;
#6852 = CARTESIAN_POINT ( 'NONE',  ( -0.09506052544073315125, -93.49547149457073658, 4.999999999999997335 ) ) ;
#6853 = CARTESIAN_POINT ( 'NONE',  ( 5.257311121191341030, -65.25452850542926342, -0.09995255151729466603 ) ) ;
#6854 = CARTESIAN_POINT ( 'NONE',  ( 2.882544866740877954, -79.39547149457074227, -0.8366430509619593447 ) ) ;
#6855 = CARTESIAN_POINT ( 'NONE',  ( -4.784657899331156372, -89.89547149457075648, 1.454677039711874675 ) ) ;
#6856 = CARTESIAN_POINT ( 'NONE',  ( 4.194503406049335581, -68.55452850542926058, -3.171033256558100089 ) ) ;
#6857 = VECTOR ( 'NONE', #5834, 1000.000000000000114 ) ;
#6858 = CARTESIAN_POINT ( 'NONE',  ( 4.191402346623198660, -85.80452850542926058, 5.607243785695311900 ) ) ;
#6859 = CARTESIAN_POINT ( 'NONE',  ( -2.610703060766923933, -96.04547149457074795, 1.773238653441125745 ) ) ;
#6860 = VERTEX_POINT ( 'NONE', #940 ) ;
#6861 = DIRECTION ( 'NONE',  ( -1.000000000000000000, 0.000000000000000000, 0.000000000000000000 ) ) ;
#6862 = EDGE_LOOP ( 'NONE', ( #8336, #3183, #1345, #6849 ) ) ;
#6863 = CARTESIAN_POINT ( 'NONE',  ( 4.725907263620341858, -92.40452850542925489, -1.635492904037697981 ) ) ;
#6864 = CARTESIAN_POINT ( 'NONE',  ( 1.840261337453269253, -64.80452850542926058, 2.371175808195547852 ) ) ;
#6865 = CARTESIAN_POINT ( 'NONE',  ( -1.719659006605370744, -93.15452850542925489, -4.969112962950016588 ) ) ;
#6866 = CARTESIAN_POINT ( 'NONE',  ( -6.686770931921459216, -74.89547149457074227, 2.072711028461789784 ) ) ;
#6867 = CARTESIAN_POINT ( 'NONE',  ( 1.719659006605392504, -94.65452850542921226, 4.969112962950016588 ) ) ;
#6868 = DIRECTION ( 'NONE',  ( -2.775557561562892337E-16, 1.000000000000000000, -0.000000000000000000 ) ) ;
#6869 = CARTESIAN_POINT ( 'NONE',  ( 2.882544866740897493, -86.10452850542924352, 0.8366430509618999478 ) ) ;
#6870 = EDGE_CURVE ( 'NONE', #6231, #4876, #7431, .T. ) ;
#6871 = PRESENTATION_STYLE_ASSIGNMENT (( #2998 ) ) ;
#6872 = VERTEX_POINT ( 'NONE', #3512 ) ;
#6873 = SURFACE_SIDE_STYLE ('',( #1272 ) ) ;
#6874 = CARTESIAN_POINT ( 'NONE',  ( 4.784657899331207886, -59.10452850542925773, 1.454677039711774533 ) ) ;
#6875 = CARTESIAN_POINT ( 'NONE',  ( 6.013306294175077227, -73.54547149457074795, -4.245374608440741326 ) ) ;
#6876 = CARTESIAN_POINT ( 'NONE',  ( 4.781359098026989329, -97.00000000000001421, -3.455279123890548032 ) ) ;
#6877 = CARTESIAN_POINT ( 'NONE',  ( 0.09506052544075525856, -76.99547149457073658, -4.999999999999997335 ) ) ;
#6878 = CARTESIAN_POINT ( 'NONE',  ( -0.09506052544073617661, -69.49547149457075079, 4.999999999999997335 ) ) ;
#6879 = CARTESIAN_POINT ( 'NONE',  ( -0.8796985632578775416, -91.35452850542925773, 3.030887037049973198 ) ) ;
#6880 = CARTESIAN_POINT ( 'NONE',  ( 65.00000000000000000, -9.999999999999994671, 10.50000000000000533 ) ) ;
#6881 = CARTESIAN_POINT ( 'NONE',  ( 4.312004677471074743, -70.95452850542925205, 3.009306630940844496 ) ) ;
#6882 = CARTESIAN_POINT ( 'NONE',  ( -0.09506052544073731458, -60.49547149457074369, 4.999999999999997335 ) ) ;
#6883 = ORIENTED_EDGE ( 'NONE', *, *, #4635, .F. ) ;
#6884 = CARTESIAN_POINT ( 'NONE',  ( -47.50000000000000711, -198.2344135219424857, 12.49999999999993960 ) ) ;
#6885 = ORIENTED_EDGE ( 'NONE', *, *, #1426, .F. ) ;
#6886 = CARTESIAN_POINT ( 'NONE',  ( 1.097606853890779561E-14, -87.00000000000001421, 0.000000000000000000 ) ) ;
#6887 = CARTESIAN_POINT ( 'NONE',  ( 0.09506052544085971667, -73.50452850542924921, 4.999999999999997335 ) ) ;
#6888 = CARTESIAN_POINT ( 'NONE',  ( 1.719659006605287033, -91.84547149457074511, -4.969112962950050338 ) ) ;
#6889 = EDGE_CURVE ( 'NONE', #7693, #5910, #4218, .T. ) ;
#6890 = CARTESIAN_POINT ( 'NONE',  ( 5.257311121191341030, -62.25452850542924210, -0.09995255151729466603 ) ) ;
#6891 = CIRCLE ( 'NONE', #5418, 5.000000000000004441 ) ;
#6892 = CARTESIAN_POINT ( 'NONE',  ( -0.8796985632579428227, -77.14547149457074227, -3.030887037049952326 ) ) ;
#6893 = CARTESIAN_POINT ( 'NONE',  ( -7.360235569667858968, -78.75452850542926342, 0.09995255151731782806 ) ) ;
#6894 = CARTESIAN_POINT ( 'NONE',  ( -4.784657899331157260, -83.89547149457074227, 1.454677039711874675 ) ) ;
#6895 = CARTESIAN_POINT ( 'NONE',  ( -4.725907263620323207, -63.90452850542925489, 1.635492904037698647 ) ) ;
#6896 = CARTESIAN_POINT ( 'NONE',  ( 5.895805022753406455, -77.55452850542926058, -4.407101234057908989 ) ) ;
#6897 = CARTESIAN_POINT ( 'NONE',  ( -0.09506052544075481447, -90.49547149457075079, 2.999999999999997780 ) ) ;
#6898 = EDGE_CURVE ( 'NONE', #3352, #7622, #6750, .T. ) ;
#6899 = ORIENTED_EDGE ( 'NONE', *, *, #8173, .F. ) ;
#6900 = LINE ( 'NONE', #5671, #5094 ) ;
#6901 = VERTEX_POINT ( 'NONE', #305 ) ;
#6902 = CARTESIAN_POINT ( 'NONE',  ( 4.194503406049340022, -89.55452850542926058, -3.171033256558100977 ) ) ;
#6903 = CARTESIAN_POINT ( 'NONE',  ( -0.09506052544082008171, -69.00452850542926342, -2.999999999999997780 ) ) ;
#6904 = CARTESIAN_POINT ( 'NONE',  ( -6.628020296210623385, -60.90452850542925489, 2.253526892787613978 ) ) ;
#6905 = AXIS2_PLACEMENT_3D ( 'NONE', #3434, #6667, #1022 ) ;
#6906 = AXIS2_PLACEMENT_3D ( 'NONE', #4239, #7448, #1635 ) ;
#6907 = CARTESIAN_POINT ( 'NONE',  ( -2.179377348189611485, -74.14547149457074227, -7.030887037049939003 ) ) ;
#6908 = CARTESIAN_POINT ( 'NONE',  ( -0.09506052544083808120, -93.00452850542926342, -4.999999999999997335 ) ) ;
#6909 = CARTESIAN_POINT ( 'NONE',  ( 0.09506052544075600796, -82.99547149457075079, -4.999999999999997335 ) ) ;
#6910 = CARTESIAN_POINT ( 'NONE',  ( -1.686450176301564241, -88.20452850542925205, 2.482926158054133303 ) ) ;
#6911 = VECTOR ( 'NONE', #8238, 1000.000000000000000 ) ;
#6912 = AXIS2_PLACEMENT_3D ( 'NONE', #7560, #3177, #3262 ) ;
#6913 = SURFACE_SIDE_STYLE ('',( #6999 ) ) ;
#6914 = STYLED_ITEM ( 'NONE', ( #5566 ), #7177 ) ;
#6915 = VERTEX_POINT ( 'NONE', #1660 ) ;
#6916 = FILL_AREA_STYLE_COLOUR ( '', #3296 ) ;
#6917 = CARTESIAN_POINT ( 'NONE',  ( 2.882544866740898826, -95.10452850542925773, 0.8366430509618999478 ) ) ;
#6918 = CARTESIAN_POINT ( 'NONE',  ( 6.628020296210686446, -70.09547149457073090, 2.253526892787472757 ) ) ;
#6919 = CARTESIAN_POINT ( 'NONE',  ( 5.396415032409674239, -97.00000000000004263, 1.209399173379465786 ) ) ;
#6920 = CARTESIAN_POINT ( 'NONE',  ( -0.09506052544073692601, -63.49547149457074369, 4.999999999999997335 ) ) ;
#6921 = CARTESIAN_POINT ( 'NONE',  ( 4.784657899331175912, -64.39547149457074227, -1.454677039711874009 ) ) ;
#6922 = AXIS2_PLACEMENT_3D ( 'NONE', #4916, #5580, #4193 ) ;
#6923 = CARTESIAN_POINT ( 'NONE',  ( 1.840261337453273249, -94.80452850542926058, 2.371175808195547852 ) ) ;
#6924 = EDGE_CURVE ( 'NONE', #5257, #981, #4259, .T. ) ;
#6925 = LINE ( 'NONE', #7049, #7985 ) ;
#6926 = CARTESIAN_POINT ( 'NONE',  ( -0.09506052544084073186, -72.00452850542926342, -4.999999999999997335 ) ) ;
#6927 = CARTESIAN_POINT ( 'NONE',  ( 6.628020296210689999, -97.09547149457074511, 2.253526892787472757 ) ) ;
#6928 = EDGE_LOOP ( 'NONE', ( #5801, #6740, #4114, #6275 ) ) ;
#6929 = DIRECTION ( 'NONE',  ( -9.251858538542971581E-17, 1.000000000000000000, 0.000000000000000000 ) ) ;
#6930 = EDGE_CURVE ( 'NONE', #6672, #5131, #3818, .T. ) ;
#6931 = ORIENTED_EDGE ( 'NONE', *, *, #7520, .F. ) ;
#6932 = LINE ( 'NONE', #5505, #3284 ) ;
#6933 = CARTESIAN_POINT ( 'NONE',  ( -4.725907263620321430, -72.90452850542925489, 1.635492904037698647 ) ) ;
#6934 = CARTESIAN_POINT ( 'NONE',  ( 5.257311121191342806, -88.24547149457073658, 0.09995255151718437925 ) ) ;
#6935 = CARTESIAN_POINT ( 'NONE',  ( -1.529537955723671683, -64.35452850542924352, 5.030887037049979860 ) ) ;
#6936 = CARTESIAN_POINT ( 'NONE',  ( -2.493201789345291797, -71.44547149457072521, -1.934965279058240561 ) ) ;
#6937 = CARTESIAN_POINT ( 'NONE',  ( 4.037591185471442579, -77.70452850542925205, -5.718994135553947977 ) ) ;
#6938 = CARTESIAN_POINT ( 'NONE',  ( -1.529537955723775156, -89.14547149457074227, -5.030887037049945221 ) ) ;
#6939 = CARTESIAN_POINT ( 'NONE',  ( -1.529537955723671239, -70.35452850542925773, 5.030887037049979860 ) ) ;
#6940 = CARTESIAN_POINT ( 'NONE',  ( 2.369498399071224615, -73.65452850542925489, 6.969112962950009482 ) ) ;
#6941 = CARTESIAN_POINT ( 'NONE',  ( 0.09506052544077742139, -85.99547149457075079, -2.999999999999997780 ) ) ;
#6942 = EDGE_CURVE ( 'NONE', #6172, #3952, #6793, .T. ) ;
#6943 = EDGE_LOOP ( 'NONE', ( #3708, #7365, #7957, #4889 ) ) ;
#6944 = DIRECTION ( 'NONE',  ( -1.000000000000000000, -0.000000000000000000, -0.000000000000000000 ) ) ;
#6945 = DIRECTION ( 'NONE',  ( 0.09506052544079829358, -0.9954714945707482388, 0.000000000000000000 ) ) ;
#6946 = EDGE_LOOP ( 'NONE', ( #1844, #4815, #234, #493 ) ) ;
#6947 = CARTESIAN_POINT ( 'NONE',  ( 4.312004677471078296, -91.95452850542926626, 3.009306630940844052 ) ) ;
#6948 = CARTESIAN_POINT ( 'NONE',  ( -0.09506052544075405120, -96.49547149457075079, 2.999999999999997780 ) ) ;
#6949 = CARTESIAN_POINT ( 'NONE',  ( -2.179377348189463603, -61.35452850542925773, 7.030887037049988741 ) ) ;
#6950 = CARTESIAN_POINT ( 'NONE',  ( 6.013306294175077227, -67.54547149457074795, -4.245374608440741326 ) ) ;
#6951 = CARTESIAN_POINT ( 'NONE',  ( 1.719659006605286367, -82.84547149457074511, -4.969112962950050338 ) ) ;
#6952 = CARTESIAN_POINT ( 'NONE',  ( 2.823794231030040791, -80.40452850542925489, -1.017458915287783316 ) ) ;
#6953 = DIRECTION ( 'NONE',  ( -0.000000000000000000, 0.7071067811865484609, 0.7071067811865465735 ) ) ;
#6954 = EDGE_CURVE ( 'NONE', #1649, #549, #7051, .T. ) ;
#6955 = ORIENTED_EDGE ( 'NONE', *, *, #4895, .F. ) ;
#6956 = FILL_AREA_STYLE_COLOUR ( '', #6244 ) ;
#6957 = CARTESIAN_POINT ( 'NONE',  ( 3.015831842038231958, -58.80452850542925347, 3.989209796945429432 ) ) ;
#6958 = CARTESIAN_POINT ( 'NONE',  ( 5.895805022753492608, -69.94547149457073942, 4.407101234057782868 ) ) ;
#6959 = SHAPE_REPRESENTATION_RELATIONSHIP ( 'NONE' , 'NONE' ,  #153, #1677 ) ;
#6960 = CARTESIAN_POINT ( 'NONE',  ( 4.479395550549687854, -97.00000000000000000, -3.869080787693377932 ) ) ;
#6961 = CARTESIAN_POINT ( 'NONE',  ( 4.784657899331175912, -61.39547149457074227, -1.454677039711874009 ) ) ;
#6962 = CARTESIAN_POINT ( 'NONE',  ( 0.09506052544073689825, -97.99547149457075079, -6.999999999999997335 ) ) ;
#6963 = CARTESIAN_POINT ( 'NONE',  ( -0.09506052544084261924, -57.00452850542924921, -4.999999999999997335 ) ) ;
#6964 = CARTESIAN_POINT ( 'NONE',  ( -80.00000000000000000, 2.168404344971008868E-15, -12.50000000000000000 ) ) ;
#6965 = AXIS2_PLACEMENT_3D ( 'NONE', #5318, #1917, #4054 ) ;
#6966 = CARTESIAN_POINT ( 'NONE',  ( -5.257311121191324155, -69.75452850542926342, 0.09995255151729526277 ) ) ;
#6967 = CARTESIAN_POINT ( 'NONE',  ( -4.191402346623055664, -96.19547149457075363, 5.607243785695398941 ) ) ;
#6968 = SURFACE_STYLE_FILL_AREA ( #2507 ) ;
#6969 = VERTEX_POINT ( 'NONE', #1024 ) ;
#6970 = CARTESIAN_POINT ( 'NONE',  ( 47.50000000000002132, -51.00000000000000711, 12.50000000000001954 ) ) ;
#6971 = SHAPE_DEFINITION_REPRESENTATION ( #563, #1613 ) ;
#6972 = ORIENTED_EDGE ( 'NONE', *, *, #1793, .F. ) ;
#6973 = CARTESIAN_POINT ( 'NONE',  ( 6.123233995736760366E-16, -26.99999999999998934, -7.000000000000000000 ) ) ;
#6974 = CARTESIAN_POINT ( 'NONE',  ( -4.725907263620320542, -78.90452850542925489, 1.635492904037698647 ) ) ;
#6975 = CARTESIAN_POINT ( 'NONE',  ( -4.312004677470991254, -90.04547149457071953, 3.009306630940933758 ) ) ;
#6976 = CARTESIAN_POINT ( 'NONE',  ( 4.194503406049335581, -59.55452850542925347, -3.171033256558100977 ) ) ;
#6977 = CARTESIAN_POINT ( 'NONE',  ( 1.686450176301635517, -72.79547149457074795, 2.482926158054096000 ) ) ;
#6978 = VECTOR ( 'NONE', #6739, 1000.000000000000000 ) ;
#6979 = CARTESIAN_POINT ( 'NONE',  ( -4.191402346623179120, -78.30452850542926058, -5.607243785695311900 ) ) ;
#6980 = CARTESIAN_POINT ( 'NONE',  ( 2.862020680886600665, -87.79547149457074795, 4.100960146803977580 ) ) ;
#6981 = CARTESIAN_POINT ( 'NONE',  ( 54.99999999999999289, -20.00000000000000000, -7.500000000000000000 ) ) ;
#6982 = CARTESIAN_POINT ( 'NONE',  ( -6.686770931921504513, -81.60452850542927195, -2.072711028461647675 ) ) ;
#6983 = AXIS2_PLACEMENT_3D ( 'NONE', #2043, #761, #5229 ) ;
#6984 = AXIS2_PLACEMENT_3D ( 'NONE', #4581, #4001, #7165 ) ;
#6985 = CARTESIAN_POINT ( 'NONE',  ( -1.069819614139473352, -87.34547149457073090, 2.969112962950044121 ) ) ;
#6986 = CIRCLE ( 'NONE', #8077, 1.500000000000001998 ) ;
#6987 = EDGE_LOOP ( 'NONE', ( #3485, #5393, #5058, #5089 ) ) ;
#6988 = DIRECTION ( 'NONE',  ( -1.000000000000000000, 0.000000000000000000, 0.000000000000000000 ) ) ;
#6989 = CARTESIAN_POINT ( 'NONE',  ( 46.73922289128223895, -17.64104216824340199, 2.500000000000000888 ) ) ;
#6990 = ORIENTED_EDGE ( 'NONE', *, *, #6954, .F. ) ;
#6991 = CARTESIAN_POINT ( 'NONE',  ( 4.784657899331211439, -89.10452850542925773, 1.454677039711774533 ) ) ;
#6992 = CARTESIAN_POINT ( 'NONE',  ( 0.09506052544077894795, -97.99547149457075079, -2.999999999999997780 ) ) ;
#6993 = AXIS2_PLACEMENT_3D ( 'NONE', #6513, #1372, #7062 ) ;
#6994 = CARTESIAN_POINT ( 'NONE',  ( 2.369498399071222838, -61.65452850542925489, 6.969112962950009482 ) ) ;
#6995 = CARTESIAN_POINT ( 'NONE',  ( -6.013306294175061240, -66.04547149457074795, 4.245374608440741326 ) ) ;
#6996 = CARTESIAN_POINT ( 'NONE',  ( 1.529537955723796472, -84.64547149457074227, 5.030887037049945221 ) ) ;
#6997 = CARTESIAN_POINT ( 'NONE',  ( 0.09506052544083844202, -73.50452850542924921, 2.999999999999997780 ) ) ;
#6998 = STYLED_ITEM ( 'NONE', ( #6802 ), #6405 ) ;
#6999 = SURFACE_STYLE_FILL_AREA ( #8184 ) ;
#7000 =( LENGTH_UNIT ( ) NAMED_UNIT ( * ) SI_UNIT ( .MILLI., .METRE. ) );
#7001 = CARTESIAN_POINT ( 'NONE',  ( -3.154386672714787565, -90.75452850542924921, 0.09995255151727280851 ) ) ;
#7002 = CARTESIAN_POINT ( 'NONE',  ( -6.686770931921460992, -65.89547149457074227, 2.072711028461789784 ) ) ;
#7003 = EDGE_CURVE ( 'NONE', #5682, #5004, #982, .T. ) ;
#7004 = LINE ( 'NONE', #7556, #1338 ) ;
#7005 = COLOUR_RGB ( '', 0.09019608, 0.27058824, 0.51372549) ;
#7006 = CARTESIAN_POINT ( 'NONE',  ( -3.015831842038130262, -66.19547149457075363, 3.989209796945492048 ) ) ;
#7007 = CARTESIAN_POINT ( 'NONE',  ( -4.784657899331160813, -59.89547149457074227, 1.454677039711874675 ) ) ;
#7008 = CARTESIAN_POINT ( 'NONE',  ( -2.610703060766962569, -93.45452850542926626, -1.773238653441072232 ) ) ;
#7009 = DIRECTION ( 'NONE',  ( 0.000000000000000000, 0.000000000000000000, 1.000000000000000000 ) ) ;
#7010 = ADVANCED_FACE ( 'NONE', ( #5528, #3549 ), #4859, .F. ) ;
#7011 = CARTESIAN_POINT ( 'NONE',  ( -1.529537955723671683, -67.35452850542925773, 5.030887037049979860 ) ) ;
#7012 = CARTESIAN_POINT ( 'NONE',  ( 5.895805022753496161, -93.94547149457073942, 4.407101234057782868 ) ) ;
#7013 = FILL_AREA_STYLE_COLOUR ( '', #8216 ) ;
#7014 = ORIENTED_EDGE ( 'NONE', *, *, #1725, .F. ) ;
#7015 = ADVANCED_FACE ( 'NONE', ( #3357 ), #1063, .F. ) ;
#7016 = DIRECTION ( 'NONE',  ( 0.000000000000000000, 0.000000000000000000, 1.000000000000000000 ) ) ;
#7017 = ORIENTED_EDGE ( 'NONE', *, *, #5942, .F. ) ;
#7018 = DIRECTION ( 'NONE',  ( 1.000000000000000000, 0.000000000000000000, -0.000000000000000000 ) ) ;
#7019 = CARTESIAN_POINT ( 'NONE',  ( 4.725907263620340970, -80.40452850542925489, -1.635492904037697981 ) ) ;
#7020 = CARTESIAN_POINT ( 'NONE',  ( -0.09506052544073352595, -90.49547149457073658, 4.999999999999997335 ) ) ;
#7021 = CARTESIAN_POINT ( 'NONE',  ( -1.719659006605374962, -57.15452850542924779, -4.969112962950015699 ) ) ;
#7022 = CARTESIAN_POINT ( 'NONE',  ( -2.823794231030040791, -74.59547149457071669, -1.017458915287723364 ) ) ;
#7023 = CARTESIAN_POINT ( 'NONE',  ( -2.369498399071206851, -75.15452850542922647, -6.969112962950009482 ) ) ;
#7024 = CARTESIAN_POINT ( 'NONE',  ( 4.784657899331179465, -88.39547149457074227, -1.454677039711874009 ) ) ;
#7025 = FACE_OUTER_BOUND ( 'NONE', #2977, .T. ) ;
#7026 = CARTESIAN_POINT ( 'NONE',  ( 5.895805022753406455, -80.55452850542926058, -4.407101234057908989 ) ) ;
#7027 = CARTESIAN_POINT ( 'NONE',  ( 1.840261337453221291, -85.69547149457073942, -2.371175808195584267 ) ) ;
#7028 = ORIENTED_EDGE ( 'NONE', *, *, #5458, .T. ) ;
#7029 = DIRECTION ( 'NONE',  ( -1.000000000000000000, 0.000000000000000000, 0.000000000000000000 ) ) ;
#7030 = CARTESIAN_POINT ( 'NONE',  ( -4.194503406049385319, -59.44547149457074653, -3.171033256558012159 ) ) ;
#7031 = PRODUCT_DEFINITION_SHAPE ( 'NONE', 'NONE',  #8347 ) ;
#7032 = ORIENTED_EDGE ( 'NONE', *, *, #5326, .T. ) ;
#7033 = CARTESIAN_POINT ( 'NONE',  ( -4.725907263620320542, -78.90452850542925489, 1.635492904037698647 ) ) ;
#7034 = CARTESIAN_POINT ( 'NONE',  ( -0.09506052544082121969, -60.00452850542925631, -2.999999999999997780 ) ) ;
#7035 = EDGE_CURVE ( 'NONE', #914, #5555, #2055, .T. ) ;
#7036 = CARTESIAN_POINT ( 'NONE',  ( 4.784657899331211439, -92.10452850542925773, 1.454677039711774533 ) ) ;
#7037 = CARTESIAN_POINT ( 'NONE',  ( -2.369498399071057637, -72.34547149457073090, 6.969112962950058332 ) ) ;
#7038 = CARTESIAN_POINT ( 'NONE',  ( -0.09506052544073428923, -84.49547149457075079, 4.999999999999997335 ) ) ;
#7039 = CARTESIAN_POINT ( 'NONE',  ( -2.610703060766964345, -78.45452850542925205, -1.773238653441072232 ) ) ;
#7040 = DIRECTION ( 'NONE',  ( 0.000000000000000000, -0.000000000000000000, 1.000000000000000000 ) ) ;
#7041 = CARTESIAN_POINT ( 'NONE',  ( 50.00000000000000000, -9.999999999999994671, 10.50000000000000533 ) ) ;
#7042 = CARTESIAN_POINT ( 'NONE',  ( 1.840261337453272805, -91.80452850542926058, 2.371175808195547852 ) ) ;
#7043 = CARTESIAN_POINT ( 'NONE',  ( -5.895805022753479285, -62.44547149457074653, -4.407101234057782868 ) ) ;
#7044 = CIRCLE ( 'NONE', #317, 1.500000000000001776 ) ;
#7045 = CARTESIAN_POINT ( 'NONE',  ( 75.00000000000000000, 80.00000000000000000, -7.500000000000000000 ) ) ;
#7046 = CARTESIAN_POINT ( 'NONE',  ( -4.725907263620355181, -62.59547149457074511, -1.635492904037597617 ) ) ;
#7047 = CARTESIAN_POINT ( 'NONE',  ( 4.194503406049400418, -63.94547149457075363, 3.171033256558012159 ) ) ;
#7048 = LINE ( 'NONE', #5862, #6844 ) ;
#7049 = CARTESIAN_POINT ( 'NONE',  ( 47.49999999999999289, -46.99999999999998579, 12.49999999999993960 ) ) ;
#7050 = STYLED_ITEM ( 'NONE', ( #2087 ), #4378 ) ;
#7051 = CIRCLE ( 'NONE', #5159, 1.500000000000000666 ) ;
#7052 = CARTESIAN_POINT ( 'NONE',  ( 2.862020680886513624, -71.70452850542925205, -4.100960146804039752 ) ) ;
#7053 = CARTESIAN_POINT ( 'NONE',  ( 6.628020296210689111, -88.09547149457074511, 2.253526892787472757 ) ) ;
#7054 = VECTOR ( 'NONE', #1412, 1000.000000000000000 ) ;
#7055 = ORIENTED_EDGE ( 'NONE', *, *, #3852, .F. ) ;
#7056 = DIRECTION ( 'NONE',  ( 0.000000000000000000, 0.000000000000000000, 1.000000000000000000 ) ) ;
#7057 = APPLICATION_PROTOCOL_DEFINITION ( 'draft international standard', 'automotive_design', 1998, #6632 ) ;
#7058 = ORIENTED_EDGE ( 'NONE', *, *, #3773, .F. ) ;
#7059 = FACE_OUTER_BOUND ( 'NONE', #2555, .T. ) ;
#7060 = CARTESIAN_POINT ( 'NONE',  ( 4.725907263620340082, -74.40452850542925489, -1.635492904037697981 ) ) ;
#7061 = CARTESIAN_POINT ( 'NONE',  ( 5.257311121191341918, -82.24547149457070816, 0.09995255151718437925 ) ) ;
#7062 = DIRECTION ( 'NONE',  ( -1.000000000000000000, 0.000000000000000000, 0.000000000000000000 ) ) ;
#7063 = CARTESIAN_POINT ( 'NONE',  ( -1.069819614139475350, -72.34547149457073090, 2.969112962950044121 ) ) ;
#7064 = CARTESIAN_POINT ( 'NONE',  ( 4.037591185471441690, -65.70452850542925205, -5.718994135553947977 ) ) ;
#7065 = CARTESIAN_POINT ( 'NONE',  ( 5.257311121191341918, -79.24547149457075079, 0.09995255151718437925 ) ) ;
#7066 = CARTESIAN_POINT ( 'NONE',  ( 4.194503406049334693, -59.55452850542926058, -3.171033256558100089 ) ) ;
#7067 = CARTESIAN_POINT ( 'NONE',  ( 2.862020680886516732, -95.70452850542926626, -4.100960146804039752 ) ) ;
#7068 = CARTESIAN_POINT ( 'NONE',  ( 6.686770931921523164, -77.10452850542924352, 2.072711028461649008 ) ) ;
#7069 = CARTESIAN_POINT ( 'NONE',  ( -0.8796985632579410463, -92.14547149457074227, -3.030887037049952326 ) ) ;
#7070 = EDGE_CURVE ( 'NONE', #2088, #6901, #6645, .T. ) ;
#7071 = ORIENTED_EDGE ( 'NONE', *, *, #2287, .F. ) ;
#7072 = CARTESIAN_POINT ( 'NONE',  ( 45.00000000000000000, -14.99999999999999467, 5.204170427930420494E-15 ) ) ;
#7073 = CARTESIAN_POINT ( 'NONE',  ( -3.015831842038131150, -60.19547149457074653, 3.989209796945492048 ) ) ;
#7074 = CARTESIAN_POINT ( 'NONE',  ( -1.719659006605370744, -87.15452850542926910, -4.969112962950016588 ) ) ;
#7075 = ORIENTED_EDGE ( 'NONE', *, *, #1919, .F. ) ;
#7076 = CARTESIAN_POINT ( 'NONE',  ( 3.015831842038233734, -76.80452850542926058, 3.989209796945429432 ) ) ;
#7077 = CARTESIAN_POINT ( 'NONE',  ( -2.610703060766967010, -60.45452850542925916, -1.773238653441072232 ) ) ;
#7078 = EDGE_CURVE ( 'NONE', #2153, #1092, #3428, .T. ) ;
#7079 = CARTESIAN_POINT ( 'NONE',  ( 4.784657899331210551, -83.10452850542927195, 1.454677039711774533 ) ) ;
#7080 = CARTESIAN_POINT ( 'NONE',  ( -2.179377348189612817, -65.14547149457074227, -7.030887037049939003 ) ) ;
#7081 = CARTESIAN_POINT ( 'NONE',  ( 4.784657899331179465, -88.39547149457074227, -1.454677039711874009 ) ) ;
#7082 = CARTESIAN_POINT ( 'NONE',  ( -0.09506052544081970701, -72.00452850542926342, -2.999999999999997780 ) ) ;
#7083 = CARTESIAN_POINT ( 'NONE',  ( 47.49999999999999289, -96.99999999999998579, 12.49999999999996803 ) ) ;
#7084 = FACE_OUTER_BOUND ( 'NONE', #5617, .T. ) ;
#7085 = CARTESIAN_POINT ( 'NONE',  ( 2.493201789345272701, -89.55452850542926058, -1.934965279058294518 ) ) ;
#7086 = CARTESIAN_POINT ( 'NONE',  ( -6.628020296210670459, -59.59547149457074511, -2.253526892787471869 ) ) ;
#7087 = CARTESIAN_POINT ( 'NONE',  ( -80.00000000000000000, 0.000000000000000000, 20.00000000000000000 ) ) ;
#7088 = CARTESIAN_POINT ( 'NONE',  ( -4.312004677470994807, -66.04547149457073374, 3.009306630940933314 ) ) ;
#7089 = CARTESIAN_POINT ( 'NONE',  ( 1.529537955723794251, -63.64547149457074227, 5.030887037049945221 ) ) ;
#7090 = CARTESIAN_POINT ( 'NONE',  ( 4.000000000000011546, -87.00000000000001421, 0.000000000000000000 ) ) ;
#7091 = DIRECTION ( 'NONE',  ( 1.000000000000000000, 9.251858538542971581E-17, 0.000000000000000000 ) ) ;
#7092 = CARTESIAN_POINT ( 'NONE',  ( 3.015831842038231958, -61.80452850542926058, 3.989209796945429432 ) ) ;
#7093 = SHAPE_REPRESENTATION ( 'High-Rigidity Aluminium Body Shell', ( #2840 ), #4982 ) ;
#7094 = CARTESIAN_POINT ( 'NONE',  ( -6.013306294175058575, -90.04547149457074795, 4.245374608440741326 ) ) ;
#7095 =( NAMED_UNIT ( * ) SI_UNIT ( $, .STERADIAN. ) SOLID_ANGLE_UNIT ( ) );
#7096 = ORIENTED_EDGE ( 'NONE', *, *, #734, .T. ) ;
#7097 = CARTESIAN_POINT ( 'NONE',  ( 4.725907263620340082, -74.40452850542925489, -1.635492904037697981 ) ) ;
#7098 = ADVANCED_FACE ( 'NONE', ( #1742 ), #3800, .F. ) ;
#7099 = FACE_OUTER_BOUND ( 'NONE', #458, .T. ) ;
#7100 = ADVANCED_BREP_SHAPE_REPRESENTATION ( '', ( #4378, #2840 ), #6190 ) ;
#7101 = CARTESIAN_POINT ( 'NONE',  ( 54.99999999999999289, -20.00000000000000000, 7.500000000000000000 ) ) ;
#7102 = CARTESIAN_POINT ( 'NONE',  ( 4.784657899331178577, -82.39547149457074227, -1.454677039711874009 ) ) ;
#7103 = CARTESIAN_POINT ( 'NONE',  ( 1.836369172260436056, -96.99999999999992895, -3.600965674691625207 ) ) ;
#7104 = CARTESIAN_POINT ( 'NONE',  ( -1.686450176301617310, -74.29547149457074795, -2.482926158054096000 ) ) ;
#7105 = CARTESIAN_POINT ( 'NONE',  ( -2.179377348189461827, -70.35452850542922931, 7.030887037049988741 ) ) ;
#7106 = DIRECTION ( 'NONE',  ( 0.000000000000000000, -2.775557561562891351E-16, 1.000000000000000000 ) ) ;
#7107 = PRODUCT_RELATED_PRODUCT_CATEGORY ( 'part', '', ( #3664 ) ) ;
#7108 = CARTESIAN_POINT ( 'NONE',  ( -4.725907263620353405, -80.59547149457074511, -1.635492904037597617 ) ) ;
#7109 = CARTESIAN_POINT ( 'NONE',  ( -0.09506052544084224454, -60.00452850542925631, -4.999999999999997335 ) ) ;
#7110 = DIRECTION ( 'NONE',  ( -0.000000000000000000, -0.000000000000000000, -1.000000000000000000 ) ) ;
#7111 = CARTESIAN_POINT ( 'NONE',  ( 5.895805022753404678, -65.55452850542926058, -4.407101234057908989 ) ) ;
#7112 = CARTESIAN_POINT ( 'NONE',  ( -0.09506052544075593858, -81.49547149457075079, 2.999999999999997780 ) ) ;
#7113 = ORIENTED_EDGE ( 'NONE', *, *, #4472, .F. ) ;
#7114 = DIRECTION ( 'NONE',  ( -1.261617073437677752E-16, 1.000000000000000000, 0.000000000000000000 ) ) ;
#7115 = DIRECTION ( 'NONE',  ( 1.000000000000000000, 0.000000000000000000, 0.000000000000000000 ) ) ;
#7116 = CARTESIAN_POINT ( 'NONE',  ( -3.015831842038213750, -84.30452850542926058, -3.989209796945429432 ) ) ;
#7117 = EDGE_LOOP ( 'NONE', ( #4516, #5047, #5217, #789 ) ) ;
#7118 = CARTESIAN_POINT ( 'NONE',  ( -1.719659006605372076, -78.15452850542926910, -4.969112962950015699 ) ) ;
#7119 = CARTESIAN_POINT ( 'NONE',  ( -3.154386672714791118, -63.75452850542926342, 0.09995255151727280851 ) ) ;
#7120 = DIRECTION ( 'NONE',  ( 1.000000000000000000, 0.000000000000000000, 0.000000000000000000 ) ) ;
#7121 = CARTESIAN_POINT ( 'NONE',  ( 4.194503406049338246, -83.55452850542921794, -3.171033256558100089 ) ) ;
#7122 = CARTESIAN_POINT ( 'NONE',  ( 6.628020296210686446, -61.09547149457074511, 2.253526892787472757 ) ) ;
#7123 = CIRCLE ( 'NONE', #6579, 1.499999999999994449 ) ;
#7124 = CARTESIAN_POINT ( 'NONE',  ( -1.529537955723776710, -80.14547149457072805, -5.030887037049945221 ) ) ;
#7125 = CARTESIAN_POINT ( 'NONE',  ( 2.493201789345271369, -77.55452850542926058, -1.934965279058294518 ) ) ;
#7126 = CYLINDRICAL_SURFACE ( 'NONE', #521, 3.000000000000000000 ) ;
#7127 = PRODUCT_DEFINITION_FORMATION_WITH_SPECIFIED_SOURCE ( 'ANY', '', #6217, .NOT_KNOWN. ) ;
#7128 = FACE_OUTER_BOUND ( 'NONE', #4557, .T. ) ;
#7129 = CARTESIAN_POINT ( 'NONE',  ( -1.069819614139537522, -84.15452850542925489, -2.969112962950023249 ) ) ;
#7130 = ADVANCED_FACE ( 'NONE', ( #4339 ), #5605, .T. ) ;
#7131 = CARTESIAN_POINT ( 'NONE',  ( 4.191402346623076980, -64.69547149457073942, -5.607243785695398941 ) ) ;
#7132 = CYLINDRICAL_SURFACE ( 'NONE', #7617, 1.500000000000000666 ) ;
#7133 = CARTESIAN_POINT ( 'NONE',  ( 0.09506052544086007750, -76.50452850542924921, 4.999999999999997335 ) ) ;
#7134 = CARTESIAN_POINT ( 'NONE',  ( -2.179377348189609265, -86.14547149457072805, -7.030887037049939003 ) ) ;
#7135 = CYLINDRICAL_SURFACE ( 'NONE', #3876, 1.499999999999994449 ) ;
#7136 = MANIFOLD_SOLID_BREP ( 'Cavity1', #6261 ) ;
#7137 = CARTESIAN_POINT ( 'NONE',  ( 6.123233995736760366E-16, -26.99999999999998934, 0.000000000000000000 ) ) ;
#7138 = CIRCLE ( 'NONE', #4561, 1.499999999999994449 ) ;
#7139 = CARTESIAN_POINT ( 'NONE',  ( -4.725907263620323207, -60.90452850542925489, 1.635492904037698647 ) ) ;
#7140 = STYLED_ITEM ( 'NONE', ( #6170 ), #3095 ) ;
#7141 = CARTESIAN_POINT ( 'NONE',  ( 5.895805022753496161, -87.94547149457073942, 4.407101234057782868 ) ) ;
#7142 = ORIENTED_EDGE ( 'NONE', *, *, #3219, .T. ) ;
#7143 = CARTESIAN_POINT ( 'NONE',  ( -1.719659006605372964, -72.15452850542921226, -4.969112962950016588 ) ) ;
#7144 = EDGE_CURVE ( 'NONE', #2822, #8028, #51, .T. ) ;
#7145 = CARTESIAN_POINT ( 'NONE',  ( 43.45299461620743386, 65.00000000000000000, 7.500000000000000000 ) ) ;
#7146 = CONTEXT_DEPENDENT_SHAPE_REPRESENTATION ( #8307, #6148 ) ;
#7147 = DIRECTION ( 'NONE',  ( -1.000000000000000000, -0.000000000000000000, -0.000000000000000000 ) ) ;
#7148 = CARTESIAN_POINT ( 'NONE',  ( -3.015831842038128485, -81.19547149457073942, 3.989209796945492048 ) ) ;
#7149 = CARTESIAN_POINT ( 'NONE',  ( 4.241803400547042635, -96.99999999999998579, 2.098537186797552412 ) ) ;
#7150 = CARTESIAN_POINT ( 'NONE',  ( -2.493201789345293129, -59.44547149457074653, -1.934965279058240561 ) ) ;
#7151 = CARTESIAN_POINT ( 'NONE',  ( -7.360235569667858968, -66.75452850542926342, 0.09995255151731782806 ) ) ;
#7152 = DIRECTION ( 'NONE',  ( 0.000000000000000000, -1.000000000000000000, 0.000000000000000000 ) ) ;
#7153 = CARTESIAN_POINT ( 'NONE',  ( -1.719659006605264828, -81.34547149457074511, 4.969112962950051227 ) ) ;
#7154 = CARTESIAN_POINT ( 'NONE',  ( -3.015831842038217303, -57.30452850542925347, -3.989209796945429432 ) ) ;
#7155 = CARTESIAN_POINT ( 'NONE',  ( -4.312004677471056091, -90.45452850542926626, -3.009306630940844052 ) ) ;
#7156 = CARTESIAN_POINT ( 'NONE',  ( -6.628020296210622497, -66.90452850542925489, 2.253526892787613978 ) ) ;
#7157 = CARTESIAN_POINT ( 'NONE',  ( -2.823794231030040791, -74.59547149457071669, -1.017458915287723364 ) ) ;
#7158 = EDGE_LOOP ( 'NONE', ( #1782, #4964, #2812, #7908 ) ) ;
#7159 = FACE_BOUND ( 'NONE', #2302, .T. ) ;
#7160 = CARTESIAN_POINT ( 'NONE',  ( -0.09506052544083808120, -93.00452850542926342, -4.999999999999997335 ) ) ;
#7161 = CARTESIAN_POINT ( 'NONE',  ( -4.725907263620320542, -84.90452850542925489, 1.635492904037698647 ) ) ;
#7162 = ORIENTED_EDGE ( 'NONE', *, *, #866, .T. ) ;
#7163 = CARTESIAN_POINT ( 'NONE',  ( 1.529537955723691223, -83.85452850542927195, -5.030887037049978971 ) ) ;
#7164 = CARTESIAN_POINT ( 'NONE',  ( -2.610703060766923933, -93.04547149457074795, 1.773238653441125745 ) ) ;
#7165 = DIRECTION ( 'NONE',  ( 0.8672199170124480494, -0.4979253112033197870, 0.000000000000000000 ) ) ;
#7166 = CARTESIAN_POINT ( 'NONE',  ( 1.529537955723691001, -83.85452850542927195, -5.030887037049978971 ) ) ;
#7167 = CARTESIAN_POINT ( 'NONE',  ( -2.369498399071059414, -60.34547149457074511, 6.969112962950058332 ) ) ;
#7168 = CARTESIAN_POINT ( 'NONE',  ( -3.154386672714791118, -63.75452850542926342, 0.09995255151727280851 ) ) ;
#7169 = LINE ( 'NONE', #5809, #126 ) ;
#7170 = LINE ( 'NONE', #261, #7401 ) ;
#7171 = CARTESIAN_POINT ( 'NONE',  ( 0.09506052544084069023, -91.50452850542926342, 2.999999999999997780 ) ) ;
#7172 = CARTESIAN_POINT ( 'NONE',  ( 6.628020296210686446, -61.09547149457074511, 2.253526892787472757 ) ) ;
#7173 = LINE ( 'NONE', #6580, #6173 ) ;
#7174 = CARTESIAN_POINT ( 'NONE',  ( -4.194503406049316929, -76.05452850542926058, 3.171033256558100533 ) ) ;
#7175 = CARTESIAN_POINT ( 'NONE',  ( 6.686770931921479644, -88.39547149457074227, -2.072711028461788896 ) ) ;
#7176 = DIRECTION ( 'NONE',  ( -0.000000000000000000, -0.000000000000000000, -1.000000000000000000 ) ) ;
#7177 = MANIFOLD_SOLID_BREP ( 'Boss-Extrude1', #2635 ) ;
#7178 = DIRECTION ( 'NONE',  ( 0.000000000000000000, -0.7071067811865484609, -0.7071067811865465735 ) ) ;
#7179 = CARTESIAN_POINT ( 'NONE',  ( 2.493201789345309116, -69.94547149457073942, 1.934965279058241006 ) ) ;
#7180 = FILL_AREA_STYLE ('',( #5150 ) ) ;
#7181 = APPLICATION_CONTEXT ( 'automotive_design' ) ;
#7182 = CARTESIAN_POINT ( 'NONE',  ( 0.09506052544073539945, -85.99547149457075079, -6.999999999999997335 ) ) ;
#7183 = EDGE_CURVE ( 'NONE', #3650, #6629, #3675, .T. ) ;
#7184 = VERTEX_POINT ( 'NONE', #3000 ) ;
#7185 = CARTESIAN_POINT ( 'NONE',  ( 3.015831842038234178, -79.80452850542926058, 3.989209796945429432 ) ) ;
#7186 = VECTOR ( 'NONE', #6868, 1000.000000000000000 ) ;
#7187 = LINE ( 'NONE', #3313, #49 ) ;
#7188 = AXIS2_PLACEMENT_3D ( 'NONE', #426, #2963, #6551 ) ;
#7189 = VECTOR ( 'NONE', #8156, 1000.000000000000000 ) ;
#7190 = CARTESIAN_POINT ( 'NONE',  ( 6.000000000000006217, -51.00000000000000711, 2.500000000000000888 ) ) ;
#7191 = CARTESIAN_POINT ( 'NONE',  ( -4.784657899331157260, -83.89547149457074227, 1.454677039711874675 ) ) ;
#7192 = LINE ( 'NONE', #6471, #1886 ) ;
#7193 = CARTESIAN_POINT ( 'NONE',  ( 0.09506052544077400746, -58.99547149457073658, -2.999999999999997780 ) ) ;
#7194 = CARTESIAN_POINT ( 'NONE',  ( 6.628020296210639373, -71.40452850542924068, -2.253526892787612645 ) ) ;
#7195 = CARTESIAN_POINT ( 'NONE',  ( 43.45299461620744808, 50.00000000000000000, 7.500000000000000000 ) ) ;
#7196 = CARTESIAN_POINT ( 'NONE',  ( 3.015831842038149357, -79.69547149457075363, -3.989209796945492048 ) ) ;
#7197 = CARTESIAN_POINT ( 'NONE',  ( 43.45299461620744808, 50.00000000000000000, 7.500000000000000000 ) ) ;
#7198 = CARTESIAN_POINT ( 'NONE',  ( -5.257311121191323267, -84.75452850542923500, 0.09995255151729526277 ) ) ;
#7199 = CARTESIAN_POINT ( 'NONE',  ( -0.09506052544086217304, -69.00452850542926342, -6.999999999999997335 ) ) ;
#7200 = VECTOR ( 'NONE', #1633, 1000.000000000000114 ) ;
#7201 = CARTESIAN_POINT ( 'NONE',  ( 1.840261337453220847, -82.69547149457073942, -2.371175808195584267 ) ) ;
#7202 = ORIENTED_EDGE ( 'NONE', *, *, #5597, .T. ) ;
#7203 = DIRECTION ( 'NONE',  ( -0.000000000000000000, 1.000000000000000000, 1.734723475976807094E-16 ) ) ;
#7204 = CARTESIAN_POINT ( 'NONE',  ( 6.123233995736760366E-16, -27.00000000000000000, 5.000000000000000000 ) ) ;
#7205 = CARTESIAN_POINT ( 'NONE',  ( -0.09506052544083921918, -84.00452850542926342, -4.999999999999997335 ) ) ;
#7206 = ORIENTED_EDGE ( 'NONE', *, *, #438, .T. ) ;
#7207 = CARTESIAN_POINT ( 'NONE',  ( 2.862020680886514512, -77.70452850542926626, -4.100960146804039752 ) ) ;
#7208 = CARTESIAN_POINT ( 'NONE',  ( 2.823794231030061663, -91.09547149457074511, 1.017458915287723809 ) ) ;
#7209 = DIRECTION ( 'NONE',  ( 1.000000000000000000, 0.000000000000000000, 0.000000000000000000 ) ) ;
#7210 = CARTESIAN_POINT ( 'NONE',  ( -1.719659006605371188, -84.15452850542925489, -4.969112962950016588 ) ) ;
#7211 = CARTESIAN_POINT ( 'NONE',  ( 7.360235569667880284, -95.25452850542926342, -0.09995255151731691212 ) ) ;
#7212 = EDGE_CURVE ( 'NONE', #1241, #996, #6246, .T. ) ;
#7213 = CARTESIAN_POINT ( 'NONE',  ( -1.686450176301566684, -70.20452850542925205, 2.482926158054133303 ) ) ;
#7214 = DIRECTION ( 'NONE',  ( -1.000000000000000000, 0.000000000000000000, 0.000000000000000000 ) ) ;
#7215 = LINE ( 'NONE', #3300, #2696 ) ;
#7216 = CARTESIAN_POINT ( 'NONE',  ( -3.154386672714789341, -78.75452850542926342, 0.09995255151727280851 ) ) ;
#7217 = CARTESIAN_POINT ( 'NONE',  ( 5.895805022753407343, -92.55452850542926058, -4.407101234057908989 ) ) ;
#7218 = LINE ( 'NONE', #5859, #2544 ) ;
#7219 = CARTESIAN_POINT ( 'NONE',  ( 2.369498399071078953, -88.84547149457073090, -6.969112962950057444 ) ) ;
#7220 = DIRECTION ( 'NONE',  ( 1.000000000000000000, 0.000000000000000000, 0.000000000000000000 ) ) ;
#7221 = DIRECTION ( 'NONE',  ( 1.000000000000000000, 2.775557561562892337E-16, 0.000000000000000000 ) ) ;
#7222 = CARTESIAN_POINT ( 'NONE',  ( 0.09506052544077554789, -70.99547149457075079, -2.999999999999997780 ) ) ;
#7223 = EDGE_CURVE ( 'NONE', #6465, #7540, #1189, .T. ) ;
#7224 = CARTESIAN_POINT ( 'NONE',  ( -4.784657899331191899, -63.60452850542925063, -1.454677039711773867 ) ) ;
#7225 = ORIENTED_EDGE ( 'NONE', *, *, #6386, .F. ) ;
#7226 = CARTESIAN_POINT ( 'NONE',  ( 4.725907263620340082, -65.40452850542925489, -1.635492904037697981 ) ) ;
#7227 = CARTESIAN_POINT ( 'NONE',  ( 0.09506052544073462229, -79.99547149457075079, -6.999999999999997335 ) ) ;
#7228 = SHAPE_REPRESENTATION_RELATIONSHIP ( 'NONE' , 'NONE' ,  #1933, #4379 ) ;
#7229 = EDGE_LOOP ( 'NONE', ( #285, #1285, #7563 ) ) ;
#7230 = CARTESIAN_POINT ( 'NONE',  ( 0.09506052544085971667, -73.50452850542924921, 4.999999999999997335 ) ) ;
#7231 = DIRECTION ( 'NONE',  ( 1.000000000000000000, -0.000000000000000000, -0.000000000000000000 ) ) ;
#7232 = CARTESIAN_POINT ( 'NONE',  ( -4.784657899331158148, -77.89547149457074227, 1.454677039711874675 ) ) ;
#7233 = LINE ( 'NONE', #2730, #2961 ) ;
#7234 = CARTESIAN_POINT ( 'NONE',  ( -3.154386672714792006, -62.74547149457073658, -0.09995255151720625064 ) ) ;
#7235 = CARTESIAN_POINT ( 'NONE',  ( 4.191402346623196884, -67.80452850542926058, 5.607243785695311900 ) ) ;
#7236 = FACE_OUTER_BOUND ( 'NONE', #5592, .T. ) ;
#7237 = CARTESIAN_POINT ( 'NONE',  ( -0.09506052544073503863, -78.49547149457073658, 4.999999999999997335 ) ) ;
#7238 =( LENGTH_UNIT ( ) NAMED_UNIT ( * ) SI_UNIT ( .MILLI., .METRE. ) );
#7239 = CARTESIAN_POINT ( 'NONE',  ( -1.529537955723669684, -82.35452850542922931, 5.030887037049979860 ) ) ;
#7240 = CARTESIAN_POINT ( 'NONE',  ( 6.628020296210639373, -65.40452850542925489, -2.253526892787612645 ) ) ;
#7241 = CARTESIAN_POINT ( 'NONE',  ( 3.154386672714809770, -82.24547149457073658, 0.09995255151720662534 ) ) ;
#7242 = ORIENTED_EDGE ( 'NONE', *, *, #527, .T. ) ;
#7243 = DIRECTION ( 'NONE',  ( 0.000000000000000000, -0.000000000000000000, -1.000000000000000000 ) ) ;
#7244 = FACE_BOUND ( 'NONE', #4206, .T. ) ;
#7245 = CARTESIAN_POINT ( 'NONE',  ( 4.725907263620341858, -89.40452850542926910, -1.635492904037697981 ) ) ;
#7246 = ORIENTED_EDGE ( 'NONE', *, *, #4149, .F. ) ;
#7247 = CARTESIAN_POINT ( 'NONE',  ( -2.862020680886494972, -73.20452850542925205, 4.100960146804039752 ) ) ;
#7248 = CARTESIAN_POINT ( 'NONE',  ( 3.154386672714811102, -94.24547149457075079, 0.09995255151720662534 ) ) ;
#7249 = CARTESIAN_POINT ( 'NONE',  ( 4.312004677471078296, -88.95452850542922363, 3.009306630940844496 ) ) ;
#7250 = CARTESIAN_POINT ( 'NONE',  ( 6.628020296210643814, -95.40452850542926910, -2.253526892787612645 ) ) ;
#7251 = CARTESIAN_POINT ( 'NONE',  ( -2.882544866740878842, -66.60452850542924352, -0.8366430509618996147 ) ) ;
#7252 = DIRECTION ( 'NONE',  ( 1.000000000000000000, 0.000000000000000000, -0.000000000000000000 ) ) ;
#7253 = CARTESIAN_POINT ( 'NONE',  ( -47.50000000000000711, -19.99999999999999645, -12.50000000000000355 ) ) ;
#7254 = CARTESIAN_POINT ( 'NONE',  ( 1.840261337453271251, -79.80452850542926058, 2.371175808195547852 ) ) ;
#7255 = CARTESIAN_POINT ( 'NONE',  ( -5.895805022753386027, -85.05452850542926058, 4.407101234057909878 ) ) ;
#7256 = VECTOR ( 'NONE', #3286, 1000.000000000000000 ) ;
#7257 = CARTESIAN_POINT ( 'NONE',  ( -4.037591185471542943, -92.29547149457074795, -5.718994135553860936 ) ) ;
#7258 = FACE_OUTER_BOUND ( 'NONE', #3285, .T. ) ;
#7259 = DIRECTION ( 'NONE',  ( 0.000000000000000000, 1.000000000000000000, 0.000000000000000000 ) ) ;
#7260 = CARTESIAN_POINT ( 'NONE',  ( 2.882544866740876621, -70.39547149457072805, -0.8366430509619593447 ) ) ;
#7261 = STYLED_ITEM ( 'NONE', ( #6871 ), #4543 ) ;
#7262 = ORIENTED_EDGE ( 'NONE', *, *, #3100, .T. ) ;
#7263 = EDGE_CURVE ( 'NONE', #6564, #3952, #7170, .T. ) ;
#7264 = CARTESIAN_POINT ( 'NONE',  ( 4.194503406049335581, -71.55452850542926058, -3.171033256558100089 ) ) ;
#7265 = CARTESIAN_POINT ( 'NONE',  ( 4.191402346623079644, -82.69547149457073942, -5.607243785695398941 ) ) ;
#7266 = ORIENTED_EDGE ( 'NONE', *, *, #508, .F. ) ;
#7267 = AXIS2_PLACEMENT_3D ( 'NONE', #758, #4505, #3255 ) ;
#7268 = CARTESIAN_POINT ( 'NONE',  ( 4.725907263620340082, -77.40452850542925489, -1.635492904037697981 ) ) ;
#7269 = CARTESIAN_POINT ( 'NONE',  ( 54.99999999999999289, 50.00000000000000000, 7.500000000000000000 ) ) ;
#7270 = ADVANCED_FACE ( 'NONE', ( #2039 ), #3967, .F. ) ;
#7271 = ITEM_DEFINED_TRANSFORMATION ( 'NONE', 'NONE', #6984,  #2840 ) ;
#7272 = CARTESIAN_POINT ( 'NONE',  ( 4.194503406049401306, -69.94547149457071100, 3.171033256558012159 ) ) ;
#7273 = FACE_OUTER_BOUND ( 'NONE', #4900, .T. ) ;
#7274 = CARTESIAN_POINT ( 'NONE',  ( 1.069819614139492669, -64.84547149457071669, -2.969112962950042789 ) ) ;
#7275 = CARTESIAN_POINT ( 'NONE',  ( -6.686770931921507177, -63.60452850542924352, -2.072711028461647675 ) ) ;
#7276 = DIRECTION ( 'NONE',  ( -9.251858538542971581E-17, 1.000000000000000000, 0.000000000000000000 ) ) ;
#7277 = PRESENTATION_STYLE_ASSIGNMENT (( #4738 ) ) ;
#7278 = CARTESIAN_POINT ( 'NONE',  ( -4.725907263620320542, -81.90452850542925489, 1.635492904037698647 ) ) ;
#7279 = CARTESIAN_POINT ( 'NONE',  ( 2.179377348189480035, -62.85452850542923642, -7.030887037049986077 ) ) ;
#7280 = CARTESIAN_POINT ( 'NONE',  ( -1.840261337453200197, -78.19547149457073942, 2.371175808195584267 ) ) ;
#7281 = ORIENTED_EDGE ( 'NONE', *, *, #974, .T. ) ;
#7282 = CYLINDRICAL_SURFACE ( 'NONE', #1804, 1.499999999999994449 ) ;
#7283 = CARTESIAN_POINT ( 'NONE',  ( 5.257311121191343695, -95.25452850542924921, -0.09995255151729465215 ) ) ;
#7284 = CARTESIAN_POINT ( 'NONE',  ( 5.257311121191341918, -77.25452850542926342, -0.09995255151729465215 ) ) ;
#7285 = ORIENTED_EDGE ( 'NONE', *, *, #3214, .F. ) ;
#7286 = CARTESIAN_POINT ( 'NONE',  ( 4.725907263620340082, -68.40452850542925489, -1.635492904037697981 ) ) ;
#7287 = CARTESIAN_POINT ( 'NONE',  ( -1.686450176301615311, -89.29547149457074795, -2.482926158054096000 ) ) ;
#7288 = CARTESIAN_POINT ( 'NONE',  ( 2.823794231030057666, -61.09547149457074511, 1.017458915287723809 ) ) ;
#7289 = CARTESIAN_POINT ( 'NONE',  ( -6.013306294175149169, -93.45452850542926626, -4.245374608440613429 ) ) ;
#7290 = CARTESIAN_POINT ( 'NONE',  ( 0.8796985632578976366, -65.85452850542924352, -3.030887037049972310 ) ) ;
#7291 =( REPRESENTATION_RELATIONSHIP ('NONE','NONE', #4188, #1933 ) REPRESENTATION_RELATIONSHIP_WITH_TRANSFORMATION ( #7271 )SHAPE_REPRESENTATION_RELATIONSHIP( ) );
#7292 = ORIENTED_EDGE ( 'NONE', *, *, #2821, .T. ) ;
#7293 = CARTESIAN_POINT ( 'NONE',  ( 65.00000000000000000, -12.00000000000000711, 12.49999999999999822 ) ) ;
#7294 = ADVANCED_FACE ( 'NONE', ( #7128 ), #5270, .T. ) ;
#7295 = DIRECTION ( 'NONE',  ( 0.000000000000000000, 1.000000000000000000, 0.000000000000000000 ) ) ;
#7296 = CARTESIAN_POINT ( 'NONE',  ( -2.882544866740876621, -81.60452850542927195, -0.8366430509618996147 ) ) ;
#7297 = CARTESIAN_POINT ( 'NONE',  ( 6.628020296210642037, -86.40452850542926910, -2.253526892787612645 ) ) ;
#7298 = CARTESIAN_POINT ( 'NONE',  ( -6.628020296210665130, -92.59547149457074511, -2.253526892787471869 ) ) ;
#7299 = CARTESIAN_POINT ( 'NONE',  ( -54.99999999999999289, -100.0000000000000000, -20.00000000000000000 ) ) ;
#7300 = CARTESIAN_POINT ( 'NONE',  ( -80.00100000000001899, -88.00000000000004263, 0.000000000000000000 ) ) ;
#7301 = CARTESIAN_POINT ( 'NONE',  ( 2.493201789345309560, -72.94547149457073942, 1.934965279058241006 ) ) ;
#7302 = UNCERTAINTY_MEASURE_WITH_UNIT (LENGTH_MEASURE( 1.000000000000000082E-05 ), #2972, 'distance_accuracy_value', 'NONE');
#7303 = FACE_OUTER_BOUND ( 'NONE', #836, .T. ) ;
#7304 = ORIENTED_EDGE ( 'NONE', *, *, #4025, .F. ) ;
#7305 = AXIS2_PLACEMENT_3D ( 'NONE', #7137, #5863, #7815 ) ;
#7306 = CARTESIAN_POINT ( 'NONE',  ( -1.529537955723671683, -67.35452850542925773, 5.030887037049979860 ) ) ;
#7307 = CARTESIAN_POINT ( 'NONE',  ( 6.628020296210687334, -76.09547149457073090, 2.253526892787472757 ) ) ;
#7308 = VERTEX_POINT ( 'NONE', #1995 ) ;
#7309 = CARTESIAN_POINT ( 'NONE',  ( 4.725907263620340082, -68.40452850542925489, -1.635492904037697981 ) ) ;
#7310 = DIRECTION ( 'NONE',  ( 0.000000000000000000, -0.7071067811865484609, 0.7071067811865465735 ) ) ;
#7311 = CARTESIAN_POINT ( 'NONE',  ( 2.862020680886598889, -69.79547149457074795, 4.100960146803977580 ) ) ;
#7312 = DIRECTION ( 'NONE',  ( 1.000000000000000000, 2.775557561562892337E-16, -0.000000000000000000 ) ) ;
#7313 = CARTESIAN_POINT ( 'NONE',  ( -1.069819614139475794, -66.34547149457073090, 2.969112962950044121 ) ) ;
#7314 = MECHANICAL_DESIGN_GEOMETRIC_PRESENTATION_REPRESENTATION (  '', ( #7050 ), #7867 ) ;
#7315 = CARTESIAN_POINT ( 'NONE',  ( -4.037591185471424815, -58.20452850542925916, 5.718994135553947977 ) ) ;
#7316 = ORIENTED_EDGE ( 'NONE', *, *, #4237, .F. ) ;
#7317 = AXIS2_PLACEMENT_3D ( 'NONE', #3144, #7018, #735 ) ;
#7318 = PRESENTATION_STYLE_ASSIGNMENT (( #2775 ) ) ;
#7319 = CARTESIAN_POINT ( 'NONE',  ( -1.719659006605371632, -81.15452850542922647, -4.969112962950016588 ) ) ;
#7320 = VECTOR ( 'NONE', #2342, 1000.000000000000000 ) ;
#7321 = AXIS2_PLACEMENT_3D ( 'NONE', #792, #4705, #6526 ) ;
#7322 = VECTOR ( 'NONE', #4032, 1000.000000000000000 ) ;
#7323 = VECTOR ( 'NONE', #6831, 1000.000000000000000 ) ;
#7324 = ORIENTED_EDGE ( 'NONE', *, *, #5026, .T. ) ;
#7325 = DIRECTION ( 'NONE',  ( 1.000000000000000000, 0.000000000000000000, 0.000000000000000000 ) ) ;
#7326 = CARTESIAN_POINT ( 'NONE',  ( -1.529537955723668796, -85.35452850542924352, 5.030887037049979860 ) ) ;
#7327 = CARTESIAN_POINT ( 'NONE',  ( -4.312004677471057867, -75.45452850542925205, -3.009306630940844052 ) ) ;
#7328 = VERTEX_POINT ( 'NONE', #2578 ) ;
#7329 = CARTESIAN_POINT ( 'NONE',  ( -3.015831842038215971, -69.30452850542926058, -3.989209796945429432 ) ) ;
#7330 = CARTESIAN_POINT ( 'NONE',  ( -2.493201789345289132, -89.44547149457073942, -1.934965279058240561 ) ) ;
#7331 = CARTESIAN_POINT ( 'NONE',  ( 1.529537955723797138, -93.64547149457074227, 5.030887037049945221 ) ) ;
#7332 = CARTESIAN_POINT ( 'NONE',  ( 4.784657899331210551, -80.10452850542925773, 1.454677039711774533 ) ) ;
#7333 = CARTESIAN_POINT ( 'NONE',  ( -6.686770931921503625, -90.60452850542925773, -2.072711028461647675 ) ) ;
#7334 = CARTESIAN_POINT ( 'NONE',  ( 3.154386672714806217, -59.25452850542926342, -0.09995255151727241993 ) ) ;
#7335 = EDGE_CURVE ( 'NONE', #2431, #6079, #5186, .T. ) ;
#7336 = EDGE_LOOP ( 'NONE', ( #4391, #505, #7461, #8278 ) ) ;
#7337 = DIRECTION ( 'NONE',  ( -1.261617073437677752E-16, 1.000000000000000000, 0.000000000000000000 ) ) ;
#7338 = LINE ( 'NONE', #7465, #534 ) ;
#7339 = CARTESIAN_POINT ( 'NONE',  ( -0.09506052544081930455, -75.00452850542926342, -2.999999999999997780 ) ) ;
#7340 = CARTESIAN_POINT ( 'NONE',  ( -5.895805022753383362, -88.05452850542926058, 4.407101234057909878 ) ) ;
#7341 = CARTESIAN_POINT ( 'NONE',  ( 2.369498399071077177, -76.84547149457073090, -6.969112962950057444 ) ) ;
#7342 = FACE_OUTER_BOUND ( 'NONE', #968, .T. ) ;
#7343 = APPLICATION_CONTEXT ( 'automotive_design' ) ;
#7344 = CARTESIAN_POINT ( 'NONE',  ( 6.000000000000004441, -27.99999999999999645, -2.499999999999999112 ) ) ;
#7345 = CARTESIAN_POINT ( 'NONE',  ( 2.493201789345308228, -63.94547149457074653, 1.934965279058241006 ) ) ;
#7346 = ORIENTED_EDGE ( 'NONE', *, *, #8097, .F. ) ;
#7347 = DIRECTION ( 'NONE',  ( -0.000000000000000000, 1.000000000000000000, 2.168404344971010594E-16 ) ) ;
#7348 = CARTESIAN_POINT ( 'NONE',  ( -3.015831842038216415, -66.30452850542926058, -3.989209796945429432 ) ) ;
#7349 = CARTESIAN_POINT ( 'NONE',  ( 5.895805022753496161, -78.94547149457073942, 4.407101234057782868 ) ) ;
#7350 = SURFACE_STYLE_USAGE ( .BOTH. , #4774 ) ;
#7351 = CARTESIAN_POINT ( 'NONE',  ( 6.000000000000011546, -100.0010000000000048, -2.499999999999999112 ) ) ;
#7352 = CARTESIAN_POINT ( 'NONE',  ( -3.015831842038128929, -78.19547149457075363, 3.989209796945492048 ) ) ;
#7353 = CARTESIAN_POINT ( 'NONE',  ( -3.015831842038216415, -66.30452850542926058, -3.989209796945429432 ) ) ;
#7354 = DIRECTION ( 'NONE',  ( 0.000000000000000000, -0.000000000000000000, 1.000000000000000000 ) ) ;
#7355 = CARTESIAN_POINT ( 'NONE',  ( 4.312004677471011682, -67.54547149457074795, -3.009306630940933314 ) ) ;
#7356 = CARTESIAN_POINT ( 'NONE',  ( 47.50000000000002132, 47.23441352194253540, -12.50000000000001954 ) ) ;
#7357 = CARTESIAN_POINT ( 'NONE',  ( 0.09506052544075753452, -94.99547149457073658, -4.999999999999997335 ) ) ;
#7358 = CARTESIAN_POINT ( 'NONE',  ( 2.369498399071222838, -61.65452850542925489, 6.969112962950009482 ) ) ;
#7359 = ORIENTED_EDGE ( 'NONE', *, *, #4017, .F. ) ;
#7360 = ORIENTED_EDGE ( 'NONE', *, *, #3963, .T. ) ;
#7361 = PLANE ( 'NONE',  #5155 ) ;
#7362 = CARTESIAN_POINT ( 'NONE',  ( -4.784657899331190123, -84.60452850542927195, -1.454677039711773867 ) ) ;
#7363 = CARTESIAN_POINT ( 'NONE',  ( 0.09506052544086084077, -82.50452850542926342, 4.999999999999997335 ) ) ;
#7364 = PRODUCT_RELATED_PRODUCT_CATEGORY ( 'part', '', ( #2525 ) ) ;
#7365 = ORIENTED_EDGE ( 'NONE', *, *, #2654, .F. ) ;
#7366 = CARTESIAN_POINT ( 'NONE',  ( 4.194503406049336469, -68.55452850542926058, -3.171033256558100977 ) ) ;
#7367 = CARTESIAN_POINT ( 'NONE',  ( -3.154386672714789341, -83.74547149457075079, -0.09995255151720625064 ) ) ;
#7368 = CARTESIAN_POINT ( 'NONE',  ( 2.862020680886601554, -93.79547149457074795, 4.100960146803977580 ) ) ;
#7369 = CARTESIAN_POINT ( 'NONE',  ( 3.015831842038234178, -79.80452850542926058, 3.989209796945429432 ) ) ;
#7370 = CARTESIAN_POINT ( 'NONE',  ( 2.179377348189483143, -89.85452850542924352, -7.030887037049986077 ) ) ;
#7371 = AXIS2_PLACEMENT_3D ( 'NONE', #5399, #3505, #7980 ) ;
#7372 = CARTESIAN_POINT ( 'NONE',  ( 0.09506052544077857325, -94.99547149457075079, -2.999999999999997780 ) ) ;
#7373 = ORIENTED_EDGE ( 'NONE', *, *, #8026, .T. ) ;
#7374 = CARTESIAN_POINT ( 'NONE',  ( -80.00000000000000000, -20.00000000000000355, 12.49999999999999645 ) ) ;
#7375 = ORIENTED_EDGE ( 'NONE', *, *, #2092, .T. ) ;
#7376 = CARTESIAN_POINT ( 'NONE',  ( 0.000000000000000000, -51.00000000000000711, 0.000000000000000000 ) ) ;
#7377 = CARTESIAN_POINT ( 'NONE',  ( -0.8796985632578788739, -79.35452850542927195, 3.030887037049973198 ) ) ;
#7378 = EDGE_CURVE ( 'NONE', #6969, #1757, #5856, .T. ) ;
#7379 = CARTESIAN_POINT ( 'NONE',  ( -7.360235569667856304, -90.75452850542924921, 0.09995255151731782806 ) ) ;
#7380 = CARTESIAN_POINT ( 'NONE',  ( -5.895805022753477509, -77.44547149457073942, -4.407101234057782868 ) ) ;
#7381 = CARTESIAN_POINT ( 'NONE',  ( -5.999999999999993783, -47.00000000000000000, -2.499999999999999112 ) ) ;
#7382 = DIRECTION ( 'NONE',  ( -0.9662349396012460678, -0.2576626505603332173, 0.000000000000000000 ) ) ;
#7383 = CARTESIAN_POINT ( 'NONE',  ( -1.840261337453251267, -81.30452850542926058, -2.371175808195547852 ) ) ;
#7384 = PRODUCT_DEFINITION_CONTEXT ( 'detailed design', #1309, 'design' ) ;
#7385 = PRESENTATION_STYLE_ASSIGNMENT (( #342 ) ) ;
#7386 = AXIS2_PLACEMENT_3D ( 'NONE', #5791, #6474, #2601 ) ;
#7387 = EDGE_CURVE ( 'NONE', #7949, #6872, #3340, .T. ) ;
#7388 = EDGE_LOOP ( 'NONE', ( #3162, #2896, #4724, #2613 ) ) ;
#7389 = DIRECTION ( 'NONE',  ( 0.000000000000000000, 0.000000000000000000, 1.000000000000000000 ) ) ;
#7390 = CARTESIAN_POINT ( 'NONE',  ( -1.719659006605373408, -69.15452850542924068, -4.969112962950016588 ) ) ;
#7391 = AXIS2_PLACEMENT_3D ( 'NONE', #2750, #7337, #1521 ) ;
#7392 = CARTESIAN_POINT ( 'NONE',  ( 6.628020296210689111, -82.09547149457075932, 2.253526892787472757 ) ) ;
#7393 = ORIENTED_EDGE ( 'NONE', *, *, #1582, .T. ) ;
#7394 = CARTESIAN_POINT ( 'NONE',  ( 4.725907263620372056, -73.09547149457074511, 1.635492904037598283 ) ) ;
#7395 = CARTESIAN_POINT ( 'NONE',  ( -4.194503406049384431, -68.44547149457073942, -3.171033256558012159 ) ) ;
#7396 = AXIS2_PLACEMENT_3D ( 'NONE', #7597, #1232, #4343 ) ;
#7397 = CARTESIAN_POINT ( 'NONE',  ( -0.09506052544084186984, -63.00452850542925631, -4.999999999999997335 ) ) ;
#7398 = CARTESIAN_POINT ( 'NONE',  ( 45.00000000000000000, -14.99999999999999467, 9.499999999999996447 ) ) ;
#7399 = STYLED_ITEM ( 'NONE', ( #3088 ), #2890 ) ;
#7400 = AXIS2_PLACEMENT_3D ( 'NONE', #3254, #3338, #7040 ) ;
#7401 = VECTOR ( 'NONE', #7808, 1000.000000000000000 ) ;
#7402 = CARTESIAN_POINT ( 'NONE',  ( -4.725907263620354293, -71.59547149457074511, -1.635492904037597617 ) ) ;
#7403 = EDGE_CURVE ( 'NONE', #4845, #97, #1355, .T. ) ;
#7404 = DIRECTION ( 'NONE',  ( -1.000000000000000000, 0.000000000000000000, 0.000000000000000000 ) ) ;
#7405 = CARTESIAN_POINT ( 'NONE',  ( -6.013306294175155386, -57.45452850542925916, -4.245374608440613429 ) ) ;
#7406 = ORIENTED_EDGE ( 'NONE', *, *, #669, .F. ) ;
#7407 = LINE ( 'NONE', #1715, #2624 ) ;
#7408 = AXIS2_PLACEMENT_3D ( 'NONE', #6150, #4715, #5438 ) ;
#7409 = ORIENTED_EDGE ( 'NONE', *, *, #52, .T. ) ;
#7410 = FACE_BOUND ( 'NONE', #2680, .T. ) ;
#7411 = CARTESIAN_POINT ( 'NONE',  ( -3.015831842038213750, -90.30452850542926058, -3.989209796945429432 ) ) ;
#7412 = CARTESIAN_POINT ( 'NONE',  ( -3.015831842038214194, -81.30452850542926058, -3.989209796945429432 ) ) ;
#7413 = ORIENTED_EDGE ( 'NONE', *, *, #6263, .F. ) ;
#7414 = CARTESIAN_POINT ( 'NONE',  ( -1.529537955723671239, -70.35452850542927195, 5.030887037049979860 ) ) ;
#7415 = CARTESIAN_POINT ( 'NONE',  ( -1.686450176301616866, -77.29547149457074795, -2.482926158054096000 ) ) ;
#7416 =( GEOMETRIC_REPRESENTATION_CONTEXT ( 3 ) GLOBAL_UNCERTAINTY_ASSIGNED_CONTEXT ( ( #2920 ) ) GLOBAL_UNIT_ASSIGNED_CONTEXT ( ( #1366, #4599, #4061 ) ) REPRESENTATION_CONTEXT ( 'NONE', 'WORKASPACE' ) );
#7417 = CARTESIAN_POINT ( 'NONE',  ( 1.686450176301633963, -60.79547149457074084, 2.482926158054096000 ) ) ;
#7418 = CARTESIAN_POINT ( 'NONE',  ( -4.312004677471058756, -66.45452850542925205, -3.009306630940844052 ) ) ;
#7419 = CARTESIAN_POINT ( 'NONE',  ( 0.09506052544088290646, -88.50452850542926342, 6.999999999999997335 ) ) ;
#7420 = CARTESIAN_POINT ( 'NONE',  ( 2.610703060766947914, -94.54547149457073374, -1.773238653441125523 ) ) ;
#7421 = ORIENTED_EDGE ( 'NONE', *, *, #3472, .F. ) ;
#7422 = LINE ( 'NONE', #6107, #3753 ) ;
#7423 = EDGE_LOOP ( 'NONE', ( #4474, #1472, #6806, #7649, #5639 ) ) ;
#7424 = PLANE ( 'NONE',  #3899 ) ;
#7425 = CARTESIAN_POINT ( 'NONE',  ( 2.493201789345270480, -68.55452850542926058, -1.934965279058294518 ) ) ;
#7426 = CARTESIAN_POINT ( 'NONE',  ( -0.09506052544071380561, -78.49547149457075079, 6.999999999999997335 ) ) ;
#7427 = DIRECTION ( 'NONE',  ( 0.000000000000000000, 1.734723475976807094E-16, -1.000000000000000000 ) ) ;
#7428 = LINE ( 'NONE', #7470, #7457 ) ;
#7429 = CARTESIAN_POINT ( 'NONE',  ( 3.154386672714809770, -83.25452850542926342, -0.09995255151727241993 ) ) ;
#7430 = ORIENTED_EDGE ( 'NONE', *, *, #102, .T. ) ;
#7431 = LINE ( 'NONE', #5450, #7869 ) ;
#7432 = CARTESIAN_POINT ( 'NONE',  ( -0.09506052544084224454, -60.00452850542925631, -4.999999999999997335 ) ) ;
#7433 = CARTESIAN_POINT ( 'NONE',  ( -4.037591185471545607, -71.29547149457074795, -5.718994135553860936 ) ) ;
#7434 =( LENGTH_UNIT ( ) NAMED_UNIT ( * ) SI_UNIT ( .MILLI., .METRE. ) );
#7435 = CARTESIAN_POINT ( 'NONE',  ( 45.00000000000000000, -9.999999999999992895, 4.499999999999999112 ) ) ;
#7436 = CARTESIAN_POINT ( 'NONE',  ( 4.194503406049403083, -78.94547149457073942, 3.171033256558012159 ) ) ;
#7437 = CARTESIAN_POINT ( 'NONE',  ( 4.194503406049401306, -69.94547149457071100, 3.171033256558012159 ) ) ;
#7438 = CARTESIAN_POINT ( 'NONE',  ( -2.862020680886495860, -64.20452850542926626, 4.100960146804039752 ) ) ;
#7439 = CARTESIAN_POINT ( 'NONE',  ( -1.739222891282244055, -24.35895783175659446, 2.500000000000000888 ) ) ;
#7440 = EDGE_CURVE ( 'NONE', #6402, #5844, #4426, .T. ) ;
#7441 = ADVANCED_FACE ( 'NONE', ( #7084 ), #4007, .T. ) ;
#7442 = CARTESIAN_POINT ( 'NONE',  ( -0.09506052544073617661, -69.49547149457075079, 4.999999999999997335 ) ) ;
#7443 = FILL_AREA_STYLE_COLOUR ( '', #4429 ) ;
#7444 = CARTESIAN_POINT ( 'NONE',  ( 4.194503406049340022, -95.55452850542921794, -3.171033256558100089 ) ) ;
#7445 = ORIENTED_EDGE ( 'NONE', *, *, #5622, .T. ) ;
#7446 = FACE_OUTER_BOUND ( 'NONE', #6484, .T. ) ;
#7447 = VERTEX_POINT ( 'NONE', #2712 ) ;
#7448 = DIRECTION ( 'NONE',  ( 0.000000000000000000, -1.734723475976807094E-16, 1.000000000000000000 ) ) ;
#7449 = CARTESIAN_POINT ( 'NONE',  ( -4.194503406049316041, -85.05452850542926058, 3.171033256558100533 ) ) ;
#7450 = VECTOR ( 'NONE', #1591, 1000.000000000000114 ) ;
#7451 = CARTESIAN_POINT ( 'NONE',  ( -1.719659006605372076, -75.15452850542925489, -4.969112962950016588 ) ) ;
#7452 = CARTESIAN_POINT ( 'NONE',  ( -4.312004677471060532, -57.45452850542925916, -3.009306630940843608 ) ) ;
#7453 = CARTESIAN_POINT ( 'NONE',  ( -2.493201789345290464, -80.44547149457073942, -1.934965279058240561 ) ) ;
#7454 = CARTESIAN_POINT ( 'NONE',  ( -3.015831842038126709, -96.19547149457075363, 3.989209796945492048 ) ) ;
#7455 = CARTESIAN_POINT ( 'NONE',  ( 2.862020680886513624, -71.70452850542925205, -4.100960146804039752 ) ) ;
#7456 = CARTESIAN_POINT ( 'NONE',  ( -2.179377348189460051, -85.35452850542924352, 7.030887037049988741 ) ) ;
#7457 = VECTOR ( 'NONE', #6747, 1000.000000000000000 ) ;
#7458 = VECTOR ( 'NONE', #2256, 1000.000000000000000 ) ;
#7459 = CARTESIAN_POINT ( 'NONE',  ( -2.882544866740855749, -95.89547149457075648, 0.8366430509619596778 ) ) ;
#7460 = APPLICATION_PROTOCOL_DEFINITION ( 'draft international standard', 'automotive_design', 1998, #3309 ) ;
#7461 = ORIENTED_EDGE ( 'NONE', *, *, #6302, .F. ) ;
#7462 = CARTESIAN_POINT ( 'NONE',  ( 47.49999999999999289, -46.99999999999998579, -12.50000000000000888 ) ) ;
#7463 = VECTOR ( 'NONE', #6385, 1000.000000000000000 ) ;
#7464 = EDGE_LOOP ( 'NONE', ( #1550, #2990, #6123, #8098 ) ) ;
#7465 = CARTESIAN_POINT ( 'NONE',  ( 75.00000000000000000, -20.00000000000000000, 7.500000000000000000 ) ) ;
#7466 = CARTESIAN_POINT ( 'NONE',  ( -3.154386672714790674, -72.75452850542926342, 0.09995255151727280851 ) ) ;
#7467 = ADVANCED_FACE ( 'NONE', ( #171 ), #1394, .F. ) ;
#7468 = CARTESIAN_POINT ( 'NONE',  ( 4.037591185471562483, -75.79547149457074795, 5.718994135553860936 ) ) ;
#7469 = CARTESIAN_POINT ( 'NONE',  ( -4.194503406049314265, -94.05452850542926058, 3.171033256558100533 ) ) ;
#7470 = CARTESIAN_POINT ( 'NONE',  ( 47.50000000000002132, 47.23441352194253540, 12.50000000000001954 ) ) ;
#7471 = CARTESIAN_POINT ( 'NONE',  ( -1.686450176301564907, -82.20452850542925205, 2.482926158054133303 ) ) ;
#7472 = DIRECTION ( 'NONE',  ( 0.000000000000000000, -0.7071067811865465735, -0.7071067811865485719 ) ) ;
#7473 = ORIENTED_EDGE ( 'NONE', *, *, #2379, .T. ) ;
#7474 = DIRECTION ( 'NONE',  ( 1.000000000000000000, 9.251858538542971581E-17, 0.000000000000000000 ) ) ;
#7475 = CARTESIAN_POINT ( 'NONE',  ( -4.784657899331191899, -60.60452850542925773, -1.454677039711773867 ) ) ;
#7476 = CARTESIAN_POINT ( 'NONE',  ( 2.369498399071077177, -73.84547149457073090, -6.969112962950057444 ) ) ;
#7477 = EDGE_CURVE ( 'NONE', #4787, #5449, #714, .T. ) ;
#7478 = DIRECTION ( 'NONE',  ( -9.251858538542971581E-17, 1.000000000000000000, 0.000000000000000000 ) ) ;
#7479 = CARTESIAN_POINT ( 'NONE',  ( -1.529537955723777820, -71.14547149457072805, -5.030887037049945221 ) ) ;
#7480 = CARTESIAN_POINT ( 'NONE',  ( -1.719659006605267049, -66.34547149457073090, 4.969112962950051227 ) ) ;
#7481 = CARTESIAN_POINT ( 'NONE',  ( -1.529537955723671905, -61.35452850542925773, 5.030887037049979860 ) ) ;
#7482 = FACE_OUTER_BOUND ( 'NONE', #1023, .T. ) ;
#7483 = CARTESIAN_POINT ( 'NONE',  ( 5.257311121191341918, -64.24547149457073658, 0.09995255151718437925 ) ) ;
#7484 = SHAPE_REPRESENTATION_RELATIONSHIP ( 'NONE' , 'NONE' ,  #7093, #6405 ) ;
#7485 = CARTESIAN_POINT ( 'NONE',  ( -4.725907263620318766, -93.90452850542925489, 1.635492904037698647 ) ) ;
#7486 = VERTEX_POINT ( 'NONE', #6453 ) ;
#7487 = UNCERTAINTY_MEASURE_WITH_UNIT (LENGTH_MEASURE( 1.000000000000000082E-05 ), #4899, 'distance_accuracy_value', 'NONE');
#7488 = CARTESIAN_POINT ( 'NONE',  ( 50.00000000000000000, -12.00000000000000711, 12.49999999999999822 ) ) ;
#7489 = ORIENTED_EDGE ( 'NONE', *, *, #3348, .T. ) ;
#7490 = CARTESIAN_POINT ( 'NONE',  ( 40.00000000000000000, -19.99999999999999645, 9.500000000000000000 ) ) ;
#7491 = CARTESIAN_POINT ( 'NONE',  ( -2.862020680886492308, -91.20452850542926626, 4.100960146804039752 ) ) ;
#7492 = CARTESIAN_POINT ( 'NONE',  ( -4.725907263620351628, -89.59547149457074511, -1.635492904037597617 ) ) ;
#7493 = CARTESIAN_POINT ( 'NONE',  ( 0.09506052544085819012, -61.50452850542925631, 4.999999999999997335 ) ) ;
#7494 = CARTESIAN_POINT ( 'NONE',  ( 1.686450176301636850, -81.79547149457074795, 2.482926158054096000 ) ) ;
#7495 = CARTESIAN_POINT ( 'NONE',  ( 1.719659006605287033, -91.84547149457074511, -4.969112962950050338 ) ) ;
#7496 = EDGE_CURVE ( 'NONE', #8124, #5131, #7215, .T. ) ;
#7497 = CARTESIAN_POINT ( 'NONE',  ( 4.312004677471074743, -70.95452850542925205, 3.009306630940844496 ) ) ;
#7498 = CARTESIAN_POINT ( 'NONE',  ( 6.628020296210642037, -92.40452850542925489, -2.253526892787612645 ) ) ;
#7499 = CARTESIAN_POINT ( 'NONE',  ( -3.154386672714792006, -60.75452850542924921, 0.09995255151727280851 ) ) ;
#7500 = ORIENTED_EDGE ( 'NONE', *, *, #5942, .T. ) ;
#7501 = CYLINDRICAL_SURFACE ( 'NONE', #1468, 1.500000000000000666 ) ;
#7502 = PRODUCT_DEFINITION_SHAPE ( 'NONE', 'NONE',  #1497 ) ;
#7503 = ORIENTED_EDGE ( 'NONE', *, *, #2429, .T. ) ;
#7504 = CARTESIAN_POINT ( 'NONE',  ( 2.862020680886515400, -86.70452850542925205, -4.100960146804039752 ) ) ;
#7505 = CARTESIAN_POINT ( 'NONE',  ( -3.154386672714790674, -69.75452850542926342, 0.09995255151727280851 ) ) ;
#7506 = CARTESIAN_POINT ( 'NONE',  ( -4.191402346623058328, -75.19547149457073942, 5.607243785695398941 ) ) ;
#7507 = DIRECTION ( 'NONE',  ( -1.000000000000000000, -1.261617073437677752E-16, 0.000000000000000000 ) ) ;
#7508 = CARTESIAN_POINT ( 'NONE',  ( -4.194503406049380878, -95.44547149457073942, -3.171033256558012159 ) ) ;
#7509 = CARTESIAN_POINT ( 'NONE',  ( -2.610703060766962569, -87.45452850542925205, -1.773238653441072232 ) ) ;
#7510 = VECTOR ( 'NONE', #4805, 1000.000000000000000 ) ;
#7511 = FILL_AREA_STYLE_COLOUR ( '', #5504 ) ;
#7512 = ORIENTED_EDGE ( 'NONE', *, *, #186, .F. ) ;
#7513 = CARTESIAN_POINT ( 'NONE',  ( -1.719659006605374962, -57.15452850542924068, -4.969112962950016588 ) ) ;
#7514 = CARTESIAN_POINT ( 'NONE',  ( 6.628020296210686446, -67.09547149457073090, 2.253526892787472757 ) ) ;
#7515 = FACE_OUTER_BOUND ( 'NONE', #3042, .T. ) ;
#7516 = CARTESIAN_POINT ( 'NONE',  ( 4.312004677471010794, -70.54547149457074795, -3.009306630940932425 ) ) ;
#7517 = CARTESIAN_POINT ( 'NONE',  ( -1.719659006605266827, -69.34547149457074511, 4.969112962950051227 ) ) ;
#7518 = CARTESIAN_POINT ( 'NONE',  ( -3.154386672714787565, -93.75452850542926342, 0.09995255151727280851 ) ) ;
#7519 = CARTESIAN_POINT ( 'NONE',  ( 50.00000000000000000, -9.999999999999994671, 0.000000000000000000 ) ) ;
#7520 = EDGE_CURVE ( 'NONE', #1162, #7447, #807, .T. ) ;
#7521 = CARTESIAN_POINT ( 'NONE',  ( 1.719659006605389173, -64.65452850542925489, 4.969112962950016588 ) ) ;
#7522 = CARTESIAN_POINT ( 'NONE',  ( -2.862020680886582458, -59.29547149457074084, -4.100960146803977580 ) ) ;
#7523 = ORIENTED_EDGE ( 'NONE', *, *, #7520, .T. ) ;
#7524 = ADVANCED_FACE ( 'NONE', ( #2751, #5312 ), #7895, .F. ) ;
#7525 = AXIS2_PLACEMENT_3D ( 'NONE', #73, #5129, #5214 ) ;
#7526 = CARTESIAN_POINT ( 'NONE',  ( 75.00000000000000000, 80.00000000000000000, 7.500000000000000000 ) ) ;
#7527 = PRODUCT_DEFINITION_FORMATION_WITH_SPECIFIED_SOURCE ( 'ANY', '', #3131, .NOT_KNOWN. ) ;
#7528 = ORIENTED_EDGE ( 'NONE', *, *, #1725, .T. ) ;
#7529 = DIRECTION ( 'NONE',  ( 1.000000000000000000, 0.000000000000000000, -0.000000000000000000 ) ) ;
#7530 = CARTESIAN_POINT ( 'NONE',  ( 1.529537955723690112, -77.85452850542922931, -5.030887037049978971 ) ) ;
#7531 = CARTESIAN_POINT ( 'NONE',  ( 1.529537955723796916, -90.64547149457075648, 5.030887037049945221 ) ) ;
#7532 = CARTESIAN_POINT ( 'NONE',  ( -5.257311121191325043, -63.75452850542925631, 0.09995255151729529053 ) ) ;
#7533 = CARTESIAN_POINT ( 'NONE',  ( 3.154386672714809770, -85.24547149457075079, 0.09995255151720662534 ) ) ;
#7534 = CARTESIAN_POINT ( 'NONE',  ( 2.179377348189482699, -80.85452850542925773, -7.030887037049986077 ) ) ;
#7535 = CARTESIAN_POINT ( 'NONE',  ( -1.719659006605264384, -84.34547149457071669, 4.969112962950051227 ) ) ;
#7536 = CARTESIAN_POINT ( 'NONE',  ( 2.862020680886512736, -65.70452850542925205, -4.100960146804039752 ) ) ;
#7537 = AXIS2_PLACEMENT_3D ( 'NONE', #7764, #7851, #130 ) ;
#7538 = CARTESIAN_POINT ( 'NONE',  ( -6.628020296210620721, -81.90452850542925489, 2.253526892787613978 ) ) ;
#7539 = CARTESIAN_POINT ( 'NONE',  ( 2.882544866740878398, -85.39547149457074227, -0.8366430509619593447 ) ) ;
#7540 = VERTEX_POINT ( 'NONE', #7253 ) ;
#7541 = DIRECTION ( 'NONE',  ( 0.000000000000000000, -0.7071067811865466846, 0.7071067811865484609 ) ) ;
#7542 = EDGE_LOOP ( 'NONE', ( #3450, #5050, #2297, #5421 ) ) ;
#7543 = CARTESIAN_POINT ( 'NONE',  ( -4.784657899331189235, -90.60452850542925773, -1.454677039711773867 ) ) ;
#7544 = CARTESIAN_POINT ( 'NONE',  ( -1.686450176301567350, -64.20452850542925205, 2.482926158054133303 ) ) ;
#7545 = CARTESIAN_POINT ( 'NONE',  ( -4.194503406049314265, -94.05452850542926058, 3.171033256558100533 ) ) ;
#7546 = CARTESIAN_POINT ( 'NONE',  ( 7.360235569667877620, -70.24547149457075079, 0.09995255151716216091 ) ) ;
#7547 = CARTESIAN_POINT ( 'NONE',  ( 4.725907263620341858, -92.40452850542925489, -1.635492904037697981 ) ) ;
#7548 = CARTESIAN_POINT ( 'NONE',  ( -4.194503406049382654, -86.44547149457072521, -3.171033256558012159 ) ) ;
#7549 = CARTESIAN_POINT ( 'NONE',  ( -0.09506052544081818045, -84.00452850542926342, -2.999999999999997780 ) ) ;
#7550 = CARTESIAN_POINT ( 'NONE',  ( -47.50000000000000711, -198.2344135219424857, 12.49999999999993960 ) ) ;
#7551 = ORIENTED_EDGE ( 'NONE', *, *, #1060, .F. ) ;
#7552 = DIRECTION ( 'NONE',  ( 0.000000000000000000, 0.000000000000000000, 1.000000000000000000 ) ) ;
#7553 = CARTESIAN_POINT ( 'NONE',  ( 5.257311121191341918, -62.25452850542924921, -0.09995255151729465215 ) ) ;
#7554 = CARTESIAN_POINT ( 'NONE',  ( -0.09506052544071491583, -69.49547149457075079, 6.999999999999997335 ) ) ;
#7555 = EDGE_CURVE ( 'NONE', #604, #5453, #1482, .T. ) ;
#7556 = CARTESIAN_POINT ( 'NONE',  ( 6.000000000000006217, -51.00000000000000711, -2.499999999999999112 ) ) ;
#7557 = CARTESIAN_POINT ( 'NONE',  ( -5.257311121191325043, -65.74547149457075079, -0.09995255151718372699 ) ) ;
#7558 = CARTESIAN_POINT ( 'NONE',  ( 3.015831842038147137, -64.69547149457075363, -3.989209796945492048 ) ) ;
#7559 = CARTESIAN_POINT ( 'NONE',  ( -3.015831842038217303, -57.30452850542925347, -3.989209796945429432 ) ) ;
#7560 = CARTESIAN_POINT ( 'NONE',  ( 47.50000000000002132, 47.23441352194253540, -12.50000000000001954 ) ) ;
#7561 = CARTESIAN_POINT ( 'NONE',  ( -2.862020680886495416, -67.20452850542925205, 4.100960146804039752 ) ) ;
#7562 = CARTESIAN_POINT ( 'NONE',  ( -2.862020680886582014, -62.29547149457074084, -4.100960146803977580 ) ) ;
#7563 = ORIENTED_EDGE ( 'NONE', *, *, #7403, .T. ) ;
#7564 = CARTESIAN_POINT ( 'NONE',  ( -5.999999999999993783, -51.00000000000000711, 2.500000000000000888 ) ) ;
#7565 = ORIENTED_EDGE ( 'NONE', *, *, #6942, .F. ) ;
#7566 = DIRECTION ( 'NONE',  ( 0.000000000000000000, 0.000000000000000000, -1.000000000000000000 ) ) ;
#7567 = CARTESIAN_POINT ( 'NONE',  ( -4.312004677471057867, -75.45452850542925205, -3.009306630940844052 ) ) ;
#7568 = CARTESIAN_POINT ( 'NONE',  ( -1.719659006605264162, -90.34547149457074511, 4.969112962950051227 ) ) ;
#7569 = CARTESIAN_POINT ( 'NONE',  ( -0.09506052544084148126, -66.00452850542926342, -4.999999999999997335 ) ) ;
#7570 = CARTESIAN_POINT ( 'NONE',  ( -2.610703060766926598, -72.04547149457074795, 1.773238653441125745 ) ) ;
#7571 = CARTESIAN_POINT ( 'NONE',  ( -0.09506052544086102118, -78.00452850542926342, -6.999999999999997335 ) ) ;
#7572 = CARTESIAN_POINT ( 'NONE',  ( -1.719659006605264384, -87.34547149457074511, 4.969112962950051227 ) ) ;
#7573 = CARTESIAN_POINT ( 'NONE',  ( -2.862020680886495416, -67.20452850542925205, 4.100960146804039752 ) ) ;
#7574 = CARTESIAN_POINT ( 'NONE',  ( 4.037591185471442579, -74.70452850542925205, -5.718994135553947977 ) ) ;
#7575 = CARTESIAN_POINT ( 'NONE',  ( -0.8796985632579418235, -86.14547149457072805, -3.030887037049952326 ) ) ;
#7576 = ADVANCED_FACE ( 'NONE', ( #5769 ), #3882, .F. ) ;
#7577 = ORIENTED_EDGE ( 'NONE', *, *, #3768, .T. ) ;
#7578 = CARTESIAN_POINT ( 'NONE',  ( -47.50000000000000711, -97.00000000000000000, 12.49999999999999112 ) ) ;
#7579 = FACE_OUTER_BOUND ( 'NONE', #5487, .T. ) ;
#7580 = EDGE_LOOP ( 'NONE', ( #2107, #3674 ) ) ;
#7581 = CARTESIAN_POINT ( 'NONE',  ( -4.312004677471056091, -87.45452850542925205, -3.009306630940843608 ) ) ;
#7582 = CARTESIAN_POINT ( 'NONE',  ( 2.610703060766981665, -58.95452850542925916, 1.773238653441072232 ) ) ;
#7583 = CARTESIAN_POINT ( 'NONE',  ( 3.015831842038236399, -94.80452850542924637, 3.989209796945429432 ) ) ;
#7584 = VECTOR ( 'NONE', #4100, 1000.000000000000000 ) ;
#7585 = AXIS2_PLACEMENT_3D ( 'NONE', #3611, #7566, #3695 ) ;
#7586 = CARTESIAN_POINT ( 'NONE',  ( 6.686770931921476979, -67.39547149457074227, -2.072711028461788896 ) ) ;
#7587 = EDGE_CURVE ( 'NONE', #5910, #425, #805, .T. ) ;
#7588 = CARTESIAN_POINT ( 'NONE',  ( -4.784657899331156372, -89.89547149457075648, 1.454677039711874675 ) ) ;
#7589 = CARTESIAN_POINT ( 'NONE',  ( -1.069819614139537967, -78.15452850542924068, -2.969112962950023249 ) ) ;
#7590 = CIRCLE ( 'NONE', #1130, 1.500000000000001776 ) ;
#7591 = DIRECTION ( 'NONE',  ( 0.000000000000000000, 0.7071067811865485719, -0.7071067811865465735 ) ) ;
#7592 = ORIENTED_EDGE ( 'NONE', *, *, #3535, .F. ) ;
#7593 = DIRECTION ( 'NONE',  ( 9.251858538542971828E-16, -1.000000000000000000, 0.000000000000000000 ) ) ;
#7594 = CARTESIAN_POINT ( 'NONE',  ( 4.725907263620339194, -59.40452850542926200, -1.635492904037697981 ) ) ;
#7595 = CARTESIAN_POINT ( 'NONE',  ( 4.191402346623077868, -70.69547149457073942, -5.607243785695398941 ) ) ;
#7596 = DIRECTION ( 'NONE',  ( 1.000000000000000000, 0.000000000000000000, 0.000000000000000000 ) ) ;
#7597 = CARTESIAN_POINT ( 'NONE',  ( 0.000000000000000000, 0.000000000000000000, -20.00000000000000000 ) ) ;
#7598 = CARTESIAN_POINT ( 'NONE',  ( -1.529537955723778486, -65.14547149457074227, -5.030887037049945221 ) ) ;
#7599 = CARTESIAN_POINT ( 'NONE',  ( -4.784657899331159925, -62.89547149457074227, 1.454677039711874675 ) ) ;
#7600 = AXIS2_PLACEMENT_3D ( 'NONE', #3367, #1461, #3990 ) ;
#7601 = CARTESIAN_POINT ( 'NONE',  ( 4.784657899331207886, -59.10452850542925773, 1.454677039711774533 ) ) ;
#7602 = DIRECTION ( 'NONE',  ( 0.000000000000000000, -1.000000000000000000, -1.734723475976807094E-16 ) ) ;
#7603 = CARTESIAN_POINT ( 'NONE',  ( 4.784657899331208775, -65.10452850542924352, 1.454677039711774533 ) ) ;
#7604 = CARTESIAN_POINT ( 'NONE',  ( 1.529537955723794251, -63.64547149457074227, 5.030887037049945221 ) ) ;
#7605 = ORIENTED_EDGE ( 'NONE', *, *, #4393, .T. ) ;
#7606 = CARTESIAN_POINT ( 'NONE',  ( 47.50000000000002132, -51.00000000000000711, 12.50000000000001954 ) ) ;
#7607 = CARTESIAN_POINT ( 'NONE',  ( -50.00000000000000000, 0.000000000000000000, 0.000000000000000000 ) ) ;
#7608 = ADVANCED_BREP_SHAPE_REPRESENTATION ( '', ( #1690, #2840 ), #1628 ) ;
#7609 = ORIENTED_EDGE ( 'NONE', *, *, #583, .T. ) ;
#7610 = DIRECTION ( 'NONE',  ( 0.000000000000000000, 0.000000000000000000, -1.000000000000000000 ) ) ;
#7611 = CARTESIAN_POINT ( 'NONE',  ( 2.862020680886514512, -77.70452850542926626, -4.100960146804039752 ) ) ;
#7612 = CARTESIAN_POINT ( 'NONE',  ( 4.194503406049402194, -84.94547149457073942, 3.171033256558012159 ) ) ;
#7613 = CARTESIAN_POINT ( 'NONE',  ( 0.09506052544085781542, -58.50452850542925631, 4.999999999999997335 ) ) ;
#7614 = CARTESIAN_POINT ( 'NONE',  ( 2.823794231030059887, -76.09547149457073090, 1.017458915287723809 ) ) ;
#7615 = CARTESIAN_POINT ( 'NONE',  ( 0.09506052544088212930, -82.50452850542926342, 6.999999999999997335 ) ) ;
#7616 = CARTESIAN_POINT ( 'NONE',  ( -4.312004677470991254, -90.04547149457071953, 3.009306630940933758 ) ) ;
#7617 = AXIS2_PLACEMENT_3D ( 'NONE', #2671, #5728, #2539 ) ;
#7618 = CARTESIAN_POINT ( 'NONE',  ( 0.09506052544085781542, -58.50452850542925631, 4.999999999999997335 ) ) ;
#7619 = CARTESIAN_POINT ( 'NONE',  ( -2.179377348189461827, -73.35452850542924352, 7.030887037049988741 ) ) ;
#7620 = CARTESIAN_POINT ( 'NONE',  ( 2.882544866740879286, -91.39547149457074227, -0.8366430509619593447 ) ) ;
#7621 = ADVANCED_FACE ( 'NONE', ( #845, #889 ), #7424, .F. ) ;
#7622 = VERTEX_POINT ( 'NONE', #928 ) ;
#7623 = DIRECTION ( 'NONE',  ( 0.000000000000000000, 2.775557561562892337E-16, -1.000000000000000000 ) ) ;
#7624 = DIRECTION ( 'NONE',  ( 0.000000000000000000, 0.000000000000000000, 1.000000000000000000 ) ) ;
#7625 = ORIENTED_EDGE ( 'NONE', *, *, #1855, .T. ) ;
#7626 = CARTESIAN_POINT ( 'NONE',  ( 4.725907263620342746, -95.40452850542925489, -1.635492904037697981 ) ) ;
#7627 = CARTESIAN_POINT ( 'NONE',  ( 1.686450176301583559, -62.70452850542925916, -2.482926158054133303 ) ) ;
#7628 = CARTESIAN_POINT ( 'NONE',  ( -6.628020296210623385, -57.90452850542925489, 2.253526892787613978 ) ) ;
#7629 = CARTESIAN_POINT ( 'NONE',  ( 6.686770931921476979, -70.39547149457072805, -2.072711028461788896 ) ) ;
#7630 = ADVANCED_FACE ( 'NONE', ( #1522 ), #2162, .F. ) ;
#7631 = CARTESIAN_POINT ( 'NONE',  ( -4.784657899331157260, -86.89547149457074227, 1.454677039711874675 ) ) ;
#7632 = CARTESIAN_POINT ( 'NONE',  ( -2.823794231030021251, -75.90452850542925489, 1.017458915287783316 ) ) ;
#7633 = CARTESIAN_POINT ( 'NONE',  ( 0.000000000000000000, -9.999999999999994671, 0.000000000000000000 ) ) ;
#7634 = EDGE_CURVE ( 'NONE', #6651, #1341, #4890, .T. ) ;
#7635 = ORIENTED_EDGE ( 'NONE', *, *, #4895, .T. ) ;
#7636 = DIRECTION ( 'NONE',  ( -8.326672684688674053E-16, 1.000000000000000000, 0.000000000000000000 ) ) ;
#7637 = CARTESIAN_POINT ( 'NONE',  ( 2.882544866740897049, -83.10452850542927195, 0.8366430509618999478 ) ) ;
#7638 = CARTESIAN_POINT ( 'NONE',  ( -6.686770931921460992, -62.89547149457074227, 2.072711028461789784 ) ) ;
#7639 = CARTESIAN_POINT ( 'NONE',  ( -54.99999999999999289, -100.0000000000000000, 20.00000000000000000 ) ) ;
#7640 = PRODUCT_DEFINITION_SHAPE ( 'NONE', 'NONE',  #5865 ) ;
#7641 = CARTESIAN_POINT ( 'NONE',  ( 5.257311121191341030, -61.24547149457074369, 0.09995255151718437925 ) ) ;
#7642 = CARTESIAN_POINT ( 'NONE',  ( -2.369498399071054529, -96.34547149457074511, 6.969112962950058332 ) ) ;
#7643 = CARTESIAN_POINT ( 'NONE',  ( -1.840261337453249491, -93.30452850542926058, -2.371175808195547852 ) ) ;
#7644 = DIRECTION ( 'NONE',  ( 0.000000000000000000, -1.000000000000000000, 0.000000000000000000 ) ) ;
#7645 = AXIS2_PLACEMENT_3D ( 'NONE', #3543, #1526, #4852 ) ;
#7646 = CARTESIAN_POINT ( 'NONE',  ( -1.529537955723670795, -73.35452850542922931, 5.030887037049979860 ) ) ;
#7647 = CARTESIAN_POINT ( 'NONE',  ( -2.179377348189608821, -95.14547149457074227, -7.030887037049939003 ) ) ;
#7648 = SURFACE_STYLE_FILL_AREA ( #560 ) ;
#7649 = ORIENTED_EDGE ( 'NONE', *, *, #6889, .T. ) ;
#7650 = DIRECTION ( 'NONE',  ( 0.000000000000000000, 8.673617379884033007E-17, 1.000000000000000000 ) ) ;
#7651 = SHAPE_DEFINITION_REPRESENTATION ( #7640, #1066 ) ;
#7652 = EDGE_CURVE ( 'NONE', #5112, #5449, #8019, .T. ) ;
#7653 = ORIENTED_EDGE ( 'NONE', *, *, #5995, .F. ) ;
#7654 = CARTESIAN_POINT ( 'NONE',  ( 80.00000000000000000, -7.999999999999996447, 12.49999999999999822 ) ) ;
#7655 = CARTESIAN_POINT ( 'NONE',  ( -5.257311121191323267, -81.75452850542926342, 0.09995255151729526277 ) ) ;
#7656 = CARTESIAN_POINT ( 'NONE',  ( -3.015831842038126709, -93.19547149457075363, 3.989209796945492048 ) ) ;
#7657 = CARTESIAN_POINT ( 'NONE',  ( 65.00000000000000000, -7.999999999999992895, -12.50000000000000178 ) ) ;
#7658 = CARTESIAN_POINT ( 'NONE',  ( 0.8796985632579613634, -72.64547149457072805, 3.030887037049952326 ) ) ;
#7659 = VECTOR ( 'NONE', #8175, 1000.000000000000000 ) ;
#7660 = CARTESIAN_POINT ( 'NONE',  ( 6.686770931921524941, -80.10452850542927195, 2.072711028461649008 ) ) ;
#7661 = CARTESIAN_POINT ( 'NONE',  ( 3.015831842038150690, -91.69547149457073942, -3.989209796945492048 ) ) ;
#7662 = DIRECTION ( 'NONE',  ( -0.000000000000000000, 0.000000000000000000, -1.000000000000000000 ) ) ;
#7663 = CARTESIAN_POINT ( 'NONE',  ( 5.895805022753406455, -74.55452850542926058, -4.407101234057908989 ) ) ;
#7664 = CARTESIAN_POINT ( 'NONE',  ( -3.154386672714787565, -89.74547149457073658, -0.09995255151720625064 ) ) ;
#7665 = AXIS2_PLACEMENT_3D ( 'NONE', #2412, #6286, #3716 ) ;
#7666 = EDGE_LOOP ( 'NONE', ( #3142, #7974, #6245, #5579 ) ) ;
#7667 = CARTESIAN_POINT ( 'NONE',  ( 46.49999999999999289, -14.99999999999999467, 4.500000000000000888 ) ) ;
#7668 = DIRECTION ( 'NONE',  ( 0.000000000000000000, 0.000000000000000000, 1.000000000000000000 ) ) ;
#7669 = EDGE_LOOP ( 'NONE', ( #2445, #3872, #7285, #1447 ) ) ;
#7670 = CARTESIAN_POINT ( 'NONE',  ( -5.257311121191321490, -93.75452850542927763, 0.09995255151729529053 ) ) ;
#7671 = CARTESIAN_POINT ( 'NONE',  ( 2.823794231030038571, -59.40452850542925489, -1.017458915287783316 ) ) ;
#7672 = AXIS2_PLACEMENT_3D ( 'NONE', #314, #3361, #5371 ) ;
#7673 = CARTESIAN_POINT ( 'NONE',  ( 1.529537955723692999, -95.85452850542922931, -5.030887037049978971 ) ) ;
#7674 = CARTESIAN_POINT ( 'NONE',  ( -5.895805022753479285, -65.44547149457075363, -4.407101234057782868 ) ) ;
#7675 = CARTESIAN_POINT ( 'NONE',  ( -5.257311121191322378, -89.74547149457072237, -0.09995255151718372699 ) ) ;
#7676 = CARTESIAN_POINT ( 'NONE',  ( 0.09506052544083881672, -76.50452850542926342, 2.999999999999997780 ) ) ;
#7677 = LINE ( 'NONE', #1909, #6978 ) ;
#7678 = DIRECTION ( 'NONE',  ( 0.000000000000000000, 0.000000000000000000, 1.000000000000000000 ) ) ;
#7679 = CARTESIAN_POINT ( 'NONE',  ( 2.823794231030041235, -86.40452850542926910, -1.017458915287783316 ) ) ;
#7680 = CARTESIAN_POINT ( 'NONE',  ( -2.179377348189612817, -65.14547149457074227, -7.030887037049939003 ) ) ;
#7681 = LINE ( 'NONE', #7723, #646 ) ;
#7682 = CARTESIAN_POINT ( 'NONE',  ( 1.529537955723793585, -60.64547149457074227, 5.030887037049945221 ) ) ;
#7683 = CARTESIAN_POINT ( 'NONE',  ( 2.862020680886597557, -60.79547149457074084, 4.100960146803977580 ) ) ;
#7684 = CARTESIAN_POINT ( 'NONE',  ( 0.09506052544084069023, -91.50452850542926342, 2.999999999999997780 ) ) ;
#7685 = FACE_OUTER_BOUND ( 'NONE', #904, .T. ) ;
#7686 = CARTESIAN_POINT ( 'NONE',  ( -4.194503406049319594, -70.05452850542923215, 3.171033256558100533 ) ) ;
#7687 = CARTESIAN_POINT ( 'NONE',  ( 4.191402346623080533, -91.69547149457075363, -5.607243785695398941 ) ) ;
#7688 = ORIENTED_EDGE ( 'NONE', *, *, #5026, .F. ) ;
#7689 = DIRECTION ( 'NONE',  ( -0.6099942813304201072, -0.7924058156930603447, 0.000000000000000000 ) ) ;
#7690 = ADVANCED_FACE ( 'NONE', ( #6660, #376 ), #4209, .F. ) ;
#7691 = EDGE_CURVE ( 'NONE', #1798, #5175, #3463, .T. ) ;
#7692 = APPLICATION_PROTOCOL_DEFINITION ( 'draft international standard', 'automotive_design', 1998, #7181 ) ;
#7693 = VERTEX_POINT ( 'NONE', #5479 ) ;
#7694 = CARTESIAN_POINT ( 'NONE',  ( 47.50000000000000000, -49.99999999999999289, 12.49999999999999289 ) ) ;
#7695 = CARTESIAN_POINT ( 'NONE',  ( 4.312004677471076519, -79.95452850542922363, 3.009306630940844496 ) ) ;
#7696 = CARTESIAN_POINT ( 'NONE',  ( 2.862020680886599333, -75.79547149457074795, 4.100960146803977580 ) ) ;
#7697 = CARTESIAN_POINT ( 'NONE',  ( -3.966234939601246623, -27.25766265056033433, 2.500000000000000888 ) ) ;
#7698 = CARTESIAN_POINT ( 'NONE',  ( -0.8796985632579433778, -74.14547149457074227, -3.030887037049952326 ) ) ;
#7699 = CARTESIAN_POINT ( 'NONE',  ( -6.628020296210620721, -75.90452850542925489, 2.253526892787613978 ) ) ;
#7700 = CARTESIAN_POINT ( 'NONE',  ( 5.257311121191341918, -82.24547149457070816, 0.09995255151718437925 ) ) ;
#7701 = CARTESIAN_POINT ( 'NONE',  ( -1.529537955723672349, -58.35452850542924352, 5.030887037049979860 ) ) ;
#7702 = CARTESIAN_POINT ( 'NONE',  ( 4.312004677471078296, -91.95452850542925205, 3.009306630940844496 ) ) ;
#7703 = CARTESIAN_POINT ( 'NONE',  ( -7.360235569667858080, -81.75452850542926342, 0.09995255151731782806 ) ) ;
#7704 = CARTESIAN_POINT ( 'NONE',  ( 2.823794231030060775, -85.09547149457075932, 1.017458915287723809 ) ) ;
#7705 = VECTOR ( 'NONE', #7259, 1000.000000000000000 ) ;
#7706 = ORIENTED_EDGE ( 'NONE', *, *, #903, .F. ) ;
#7707 = DIRECTION ( 'NONE',  ( 0.000000000000000000, 3.469446951953615175E-16, 1.000000000000000000 ) ) ;
#7708 = DIRECTION ( 'NONE',  ( -0.000000000000000000, 1.000000000000000000, -1.734723475976806108E-16 ) ) ;
#7709 = CARTESIAN_POINT ( 'NONE',  ( -5.257311121191322378, -87.75452850542922079, 0.09995255151729526277 ) ) ;
#7710 = ORIENTED_EDGE ( 'NONE', *, *, #3440, .T. ) ;
#7711 = CARTESIAN_POINT ( 'NONE',  ( 3.015831842038235067, -85.80452850542926058, 3.989209796945429432 ) ) ;
#7712 = CARTESIAN_POINT ( 'NONE',  ( -1.069819614139540187, -63.15452850542925489, -2.969112962950023249 ) ) ;
#7713 = CARTESIAN_POINT ( 'NONE',  ( 2.179377348189479591, -59.85452850542925773, -7.030887037049986077 ) ) ;
#7714 = CARTESIAN_POINT ( 'NONE',  ( 5.895805022753492608, -72.94547149457073942, 4.407101234057782868 ) ) ;
#7715 = CARTESIAN_POINT ( 'NONE',  ( 4.194503406049403083, -84.94547149457073942, 3.171033256558012159 ) ) ;
#7716 = CARTESIAN_POINT ( 'NONE',  ( -1.686450176301566017, -73.20452850542925205, 2.482926158054133303 ) ) ;
#7717 = CARTESIAN_POINT ( 'NONE',  ( 80.00000000000000000, -2.168404344971008868E-15, 12.50000000000000000 ) ) ;
#7718 = EDGE_CURVE ( 'NONE', #6070, #8322, #7338, .T. ) ;
#7719 = DIRECTION ( 'NONE',  ( 0.000000000000000000, -0.7071067811865484609, 0.7071067811865465735 ) ) ;
#7720 = CARTESIAN_POINT ( 'NONE',  ( 2.493201789345272701, -86.55452850542926058, -1.934965279058294518 ) ) ;
#7721 = CARTESIAN_POINT ( 'NONE',  ( 5.895805022753492608, -60.94547149457074653, 4.407101234057782868 ) ) ;
#7722 = VECTOR ( 'NONE', #5075, 1000.000000000000000 ) ;
#7723 = CARTESIAN_POINT ( 'NONE',  ( 43.45299461620744808, 50.00000000000000000, -7.500000000000000000 ) ) ;
#7724 = CARTESIAN_POINT ( 'NONE',  ( 2.862020680886598445, -66.79547149457073374, 4.100960146803977580 ) ) ;
#7725 = CARTESIAN_POINT ( 'NONE',  ( 6.686770931921480532, -97.39547149457074227, -2.072711028461788896 ) ) ;
#7726 = CYLINDRICAL_SURFACE ( 'NONE', #5211, 1.499999999999994449 ) ;
#7727 = CARTESIAN_POINT ( 'NONE',  ( -47.50000000000000711, 47.23441352194253540, 12.50000000000001954 ) ) ;
#7728 = STYLED_ITEM ( 'NONE', ( #3470 ), #4458 ) ;
#7729 = AXIS2_PLACEMENT_3D ( 'NONE', #7041, #1910, #5017 ) ;
#7730 = CARTESIAN_POINT ( 'NONE',  ( -0.09506052544084261924, -57.00452850542924921, -4.999999999999997335 ) ) ;
#7731 = ADVANCED_FACE ( 'NONE', ( #3424 ), #6028, .T. ) ;
#7732 = CARTESIAN_POINT ( 'NONE',  ( 4.037591185471564259, -93.79547149457076216, 5.718994135553860936 ) ) ;
#7733 = VECTOR ( 'NONE', #523, 1000.000000000000000 ) ;
#7734 = VERTEX_POINT ( 'NONE', #7935 ) ;
#7735 = CARTESIAN_POINT ( 'NONE',  ( 1.719659006605391172, -76.65452850542922647, 4.969112962950016588 ) ) ;
#7736 = CARTESIAN_POINT ( 'NONE',  ( 6.000000000000006217, -51.00000000000000711, 2.500000000000000888 ) ) ;
#7737 = CONTEXT_DEPENDENT_SHAPE_REPRESENTATION ( #7291, #4466 ) ;
#7738 = CARTESIAN_POINT ( 'NONE',  ( 47.49999999999999289, -96.99999999999998579, 12.49999999999993960 ) ) ;
#7739 = CARTESIAN_POINT ( 'NONE',  ( 4.784657899331177688, -79.39547149457074227, -1.454677039711874009 ) ) ;
#7740 = CARTESIAN_POINT ( 'NONE',  ( 0.09506052544075295485, -58.99547149457073658, -4.999999999999997335 ) ) ;
#7741 = CARTESIAN_POINT ( 'NONE',  ( -2.882544866740858414, -74.89547149457074227, 0.8366430509619596778 ) ) ;
#7742 = CARTESIAN_POINT ( 'NONE',  ( 2.179377348189480923, -68.85452850542924352, -7.030887037049986077 ) ) ;
#7743 = CARTESIAN_POINT ( 'NONE',  ( 80.00000000000000000, -19.99999999999999645, -12.50000000000000355 ) ) ;
#7744 = CARTESIAN_POINT ( 'NONE',  ( -2.862020680886580237, -80.29547149457074795, -4.100960146803977580 ) ) ;
#7745 = CARTESIAN_POINT ( 'NONE',  ( 4.725907263620339194, -62.40452850542925489, -1.635492904037697981 ) ) ;
#7746 = LINE ( 'NONE', #3195, #3058 ) ;
#7747 = CARTESIAN_POINT ( 'NONE',  ( 2.369498399071224171, -67.65452850542925489, 6.969112962950009482 ) ) ;
#7748 = CARTESIAN_POINT ( 'NONE',  ( -2.882544866740858414, -74.89547149457074227, 0.8366430509619596778 ) ) ;
#7749 = EDGE_CURVE ( 'NONE', #5636, #5645, #7976, .T. ) ;
#7750 = ORIENTED_EDGE ( 'NONE', *, *, #1659, .T. ) ;
#7751 = DIRECTION ( 'NONE',  ( -1.000000000000000000, -9.251858538542971581E-17, 0.000000000000000000 ) ) ;
#7752 = CARTESIAN_POINT ( 'NONE',  ( 50.00000000000000000, -9.999999999999994671, 1.500000000000000666 ) ) ;
#7753 = CARTESIAN_POINT ( 'NONE',  ( -4.312004677471056091, -87.45452850542925205, -3.009306630940844052 ) ) ;
#7754 = ORIENTED_EDGE ( 'NONE', *, *, #3269, .F. ) ;
#7755 = CARTESIAN_POINT ( 'NONE',  ( 0.09506052544086046607, -79.50452850542926342, 4.999999999999997335 ) ) ;
#7756 = CARTESIAN_POINT ( 'NONE',  ( 1.069819614139497332, -97.84547149457073090, -2.969112962950042789 ) ) ;
#7757 = EDGE_CURVE ( 'NONE', #1139, #4707, #252, .T. ) ;
#7758 =( NAMED_UNIT ( * ) SI_UNIT ( $, .STERADIAN. ) SOLID_ANGLE_UNIT ( ) );
#7759 = CARTESIAN_POINT ( 'NONE',  ( 4.194503406049339134, -86.55452850542926058, -3.171033256558100089 ) ) ;
#7760 = CARTESIAN_POINT ( 'NONE',  ( -5.895805022753480173, -59.44547149457074653, -4.407101234057782868 ) ) ;
#7761 = CARTESIAN_POINT ( 'NONE',  ( -5.257311121191325043, -80.74547149457075079, -0.09995255151718372699 ) ) ;
#7762 = CARTESIAN_POINT ( 'NONE',  ( -1.069819614139538411, -75.15452850542922647, -2.969112962950023249 ) ) ;
#7763 = CARTESIAN_POINT ( 'NONE',  ( 65.00000000000000000, -7.999999999999992895, -12.50000000000000178 ) ) ;
#7764 = CARTESIAN_POINT ( 'NONE',  ( 0.000000000000000000, 0.000000000000000000, -30.00000000000000000 ) ) ;
#7765 = CARTESIAN_POINT ( 'NONE',  ( 2.610703060766985217, -88.95452850542925205, 1.773238653441072232 ) ) ;
#7766 = CARTESIAN_POINT ( 'NONE',  ( 6.628020296210643814, -95.40452850542926910, -2.253526892787612645 ) ) ;
#7767 = DIRECTION ( 'NONE',  ( -1.000000000000000000, 0.000000000000000000, 0.000000000000000000 ) ) ;
#7768 = CARTESIAN_POINT ( 'NONE',  ( -1.529537955723670128, -79.35452850542925773, 5.030887037049979860 ) ) ;
#7769 = CARTESIAN_POINT ( 'NONE',  ( 6.013306294175080779, -94.54547149457073374, -4.245374608440741326 ) ) ;
#7770 = PLANE ( 'NONE',  #6563 ) ;
#7771 = DIRECTION ( 'NONE',  ( -1.261617073437677752E-16, 1.000000000000000000, 0.000000000000000000 ) ) ;
#7772 = CARTESIAN_POINT ( 'NONE',  ( 4.194503406049334693, -62.55452850542925347, -3.171033256558100089 ) ) ;
#7773 = APPLICATION_CONTEXT ( 'automotive_design' ) ;
#7774 = CARTESIAN_POINT ( 'NONE',  ( 0.09506052544073653743, -94.99547149457075079, -6.999999999999997335 ) ) ;
#7775 =( NAMED_UNIT ( * ) SI_UNIT ( $, .STERADIAN. ) SOLID_ANGLE_UNIT ( ) );
#7776 = EDGE_LOOP ( 'NONE', ( #7225, #561, #3454, #1207 ) ) ;
#7777 = VECTOR ( 'NONE', #7110, 1000.000000000000000 ) ;
#7778 = CARTESIAN_POINT ( 'NONE',  ( -1.529537955723670795, -73.35452850542922931, 5.030887037049979860 ) ) ;
#7779 = DIRECTION ( 'NONE',  ( 1.000000000000000000, 8.326672684688674053E-16, -0.000000000000000000 ) ) ;
#7780 = DIRECTION ( 'NONE',  ( 0.000000000000000000, 0.000000000000000000, 1.000000000000000000 ) ) ;
#7781 = CARTESIAN_POINT ( 'NONE',  ( -1.719659006605265050, -78.34547149457074511, 4.969112962950051227 ) ) ;
#7782 = EDGE_CURVE ( 'NONE', #4574, #1966, #2285, .T. ) ;
#7783 = CARTESIAN_POINT ( 'NONE',  ( 3.182720709228878064, -96.99999999999995737, -2.580399204195190865 ) ) ;
#7784 = CARTESIAN_POINT ( 'NONE',  ( -1.840261337453201973, -66.19547149457073942, 2.371175808195584267 ) ) ;
#7785 = CARTESIAN_POINT ( 'NONE',  ( -2.369498399071207739, -69.15452850542926910, -6.969112962950009482 ) ) ;
#7786 = CARTESIAN_POINT ( 'NONE',  ( 75.00000000000000000, -9.999999999999994671, 0.000000000000000000 ) ) ;
#7787 = CARTESIAN_POINT ( 'NONE',  ( -4.725907263620353405, -77.59547149457074511, -1.635492904037597617 ) ) ;
#7788 = CARTESIAN_POINT ( 'NONE',  ( -4.784657899331191899, -60.60452850542925773, -1.454677039711773867 ) ) ;
#7789 = CARTESIAN_POINT ( 'NONE',  ( 4.784657899331211439, -86.10452850542925773, 1.454677039711774533 ) ) ;
#7790 = CARTESIAN_POINT ( 'NONE',  ( 4.037591185471441690, -68.70452850542925205, -5.718994135553947977 ) ) ;
#7791 = CARTESIAN_POINT ( 'NONE',  ( -2.610703060766926153, -78.04547149457074795, 1.773238653441125745 ) ) ;
#7792 = VERTEX_POINT ( 'NONE', #3501 ) ;
#7793 = VECTOR ( 'NONE', #6988, 1000.000000000000000 ) ;
#7794 = CARTESIAN_POINT ( 'NONE',  ( 50.00000000000000000, -7.999999999999996447, 12.49999999999999822 ) ) ;
#7795 = CARTESIAN_POINT ( 'NONE',  ( 4.000000000000011546, -87.00000000000001421, 0.000000000000000000 ) ) ;
#7796 = CARTESIAN_POINT ( 'NONE',  ( 4.725907263620341858, -86.40452850542926910, -1.635492904037697981 ) ) ;
#7797 = EDGE_LOOP ( 'NONE', ( #6287, #3224, #3331, #7316 ) ) ;
#7798 = CARTESIAN_POINT ( 'NONE',  ( -1.719659006605371410, -84.15452850542925489, -4.969112962950015699 ) ) ;
#7799 = CARTESIAN_POINT ( 'NONE',  ( 1.069819614139495556, -85.84547149457074511, -2.969112962950042789 ) ) ;
#7800 = DIRECTION ( 'NONE',  ( 0.000000000000000000, 0.000000000000000000, -1.000000000000000000 ) ) ;
#7801 = CARTESIAN_POINT ( 'NONE',  ( 4.725907263620341858, -89.40452850542926910, -1.635492904037697981 ) ) ;
#7802 = CARTESIAN_POINT ( 'NONE',  ( -6.628020296210670459, -59.59547149457074511, -2.253526892787471869 ) ) ;
#7803 = AXIS2_PLACEMENT_3D ( 'NONE', #1354, #6451, #4586 ) ;
#7804 = CARTESIAN_POINT ( 'NONE',  ( -2.823794231030022139, -66.90452850542925489, 1.017458915287783316 ) ) ;
#7805 = EDGE_CURVE ( 'NONE', #6387, #6915, #5242, .T. ) ;
#7806 = FACE_OUTER_BOUND ( 'NONE', #3126, .T. ) ;
#7807 = PRODUCT_DEFINITION_FORMATION_WITH_SPECIFIED_SOURCE ( 'ANY', '', #4128, .NOT_KNOWN. ) ;
#7808 = DIRECTION ( 'NONE',  ( -0.000000000000000000, -0.000000000000000000, -1.000000000000000000 ) ) ;
#7809 = CARTESIAN_POINT ( 'NONE',  ( 0.8796985632579006342, -89.85452850542924352, -3.030887037049972310 ) ) ;
#7810 = CARTESIAN_POINT ( 'NONE',  ( 4.037591185471560706, -63.79547149457074084, 5.718994135553860936 ) ) ;
#7811 = DIRECTION ( 'NONE',  ( 1.000000000000000000, 0.000000000000000000, 0.000000000000000000 ) ) ;
#7812 = CARTESIAN_POINT ( 'NONE',  ( -4.784657899331190123, -81.60452850542925773, -1.454677039711773867 ) ) ;
#7813 = CARTESIAN_POINT ( 'NONE',  ( 6.013306294175080779, -88.54547149457074795, -4.245374608440741326 ) ) ;
#7814 = DIRECTION ( 'NONE',  ( 0.000000000000000000, -1.000000000000000000, -1.734723475976807094E-16 ) ) ;
#7815 = DIRECTION ( 'NONE',  ( 1.000000000000000000, 0.000000000000000000, -0.000000000000000000 ) ) ;
#7816 = VECTOR ( 'NONE', #3211, 1000.000000000000000 ) ;
#7817 = CARTESIAN_POINT ( 'NONE',  ( -1.069819614139475794, -69.34547149457073090, 2.969112962950044121 ) ) ;
#7818 = SURFACE_STYLE_FILL_AREA ( #7180 ) ;
#7819 = ADVANCED_FACE ( 'NONE', ( #2246 ), #4801, .T. ) ;
#7820 =( GEOMETRIC_REPRESENTATION_CONTEXT ( 3 ) GLOBAL_UNCERTAINTY_ASSIGNED_CONTEXT ( ( #3433 ) ) GLOBAL_UNIT_ASSIGNED_CONTEXT ( ( #1797, #4871, #1712 ) ) REPRESENTATION_CONTEXT ( 'NONE', 'WORKASPACE' ) );
#7821 = CARTESIAN_POINT ( 'NONE',  ( -6.686770931921456551, -89.89547149457074227, 2.072711028461789784 ) ) ;
#7822 = ORIENTED_EDGE ( 'NONE', *, *, #3661, .F. ) ;
#7823 = CARTESIAN_POINT ( 'NONE',  ( -4.784657899331190123, -72.60452850542925773, -1.454677039711773867 ) ) ;
#7824 = CYLINDRICAL_SURFACE ( 'NONE', #6241, 1.499999999999999556 ) ;
#7825 = ITEM_DEFINED_TRANSFORMATION ( 'NONE', 'NONE', #3094,  #2840 ) ;
#7826 = LINE ( 'NONE', #6080, #1122 ) ;
#7827 = CARTESIAN_POINT ( 'NONE',  ( 1.529537955723795584, -81.64547149457074227, 5.030887037049945221 ) ) ;
#7828 = EDGE_CURVE ( 'NONE', #6384, #4976, #2798, .T. ) ;
#7829 = CARTESIAN_POINT ( 'NONE',  ( 4.245875450176646915, -97.00000000000000000, 2.474278829614704467 ) ) ;
#7830 = CARTESIAN_POINT ( 'NONE',  ( -1.686450176301618864, -62.29547149457074084, -2.482926158054096000 ) ) ;
#7831 = CARTESIAN_POINT ( 'NONE',  ( 6.686770931921523164, -74.10452850542924352, 2.072711028461649008 ) ) ;
#7832 = CARTESIAN_POINT ( 'NONE',  ( 43.50000000000000711, -14.99999999999999467, 2.500000000000000888 ) ) ;
#7833 = CARTESIAN_POINT ( 'NONE',  ( 0.09506052544075563326, -79.99547149457075079, -4.999999999999997335 ) ) ;
#7834 = DIRECTION ( 'NONE',  ( -0.000000000000000000, 1.000000000000000000, 1.734723475976807094E-16 ) ) ;
#7835 = CARTESIAN_POINT ( 'NONE',  ( 2.862020680886515844, -89.70452850542926626, -4.100960146804039752 ) ) ;
#7836 = CARTESIAN_POINT ( 'NONE',  ( -2.179377348189462271, -67.35452850542924352, 7.030887037049988741 ) ) ;
#7837 = CARTESIAN_POINT ( 'NONE',  ( -0.8796985632579433778, -74.14547149457074227, -3.030887037049952326 ) ) ;
#7838 = EDGE_LOOP ( 'NONE', ( #3083, #8032 ) ) ;
#7839 = LINE ( 'NONE', #1258, #6448 ) ;
#7840 = CARTESIAN_POINT ( 'NONE',  ( -0.09506052544083770650, -96.00452850542926342, -4.999999999999997335 ) ) ;
#7841 = CARTESIAN_POINT ( 'NONE',  ( -0.09506052544083884448, -87.00452850542924921, -4.999999999999997335 ) ) ;
#7842 = ORIENTED_EDGE ( 'NONE', *, *, #4750, .T. ) ;
#7843 = CARTESIAN_POINT ( 'NONE',  ( -1.529537955723669018, -85.35452850542925773, 5.030887037049979860 ) ) ;
#7844 = CARTESIAN_POINT ( 'NONE',  ( -2.882544866740855749, -92.89547149457074227, 0.8366430509619596778 ) ) ;
#7845 = DIRECTION ( 'NONE',  ( 1.000000000000000000, 0.000000000000000000, 0.000000000000000000 ) ) ;
#7846 = CARTESIAN_POINT ( 'NONE',  ( 1.529537955723691889, -86.85452850542921510, -5.030887037049978971 ) ) ;
#7847 = ADVANCED_FACE ( 'NONE', ( #1248 ), #4482, .T. ) ;
#7848 = CARTESIAN_POINT ( 'NONE',  ( -6.686770931921460992, -62.89547149457074227, 2.072711028461789784 ) ) ;
#7849 = CARTESIAN_POINT ( 'NONE',  ( 1.686450176301583559, -62.70452850542925916, -2.482926158054133303 ) ) ;
#7850 = DIRECTION ( 'NONE',  ( 1.000000000000000000, 0.000000000000000000, 0.000000000000000000 ) ) ;
#7851 = DIRECTION ( 'NONE',  ( 0.000000000000000000, 0.000000000000000000, -1.000000000000000000 ) ) ;
#7852 = CARTESIAN_POINT ( 'NONE',  ( 2.610703060766984329, -82.95452850542925205, 1.773238653441072232 ) ) ;
#7853 = CARTESIAN_POINT ( 'NONE',  ( -2.369498399071205075, -90.15452850542926910, -6.969112962950009482 ) ) ;
#7854 = FACE_BOUND ( 'NONE', #6422, .T. ) ;
#7855 = CARTESIAN_POINT ( 'NONE',  ( 2.179377348189630137, -84.64547149457074227, 7.030887037049939003 ) ) ;
#7856 = CARTESIAN_POINT ( 'NONE',  ( 45.00000000000000000, -14.99999999999999467, 4.500000000000000888 ) ) ;
#7857 = FACE_OUTER_BOUND ( 'NONE', #6135, .T. ) ;
#7858 = EDGE_CURVE ( 'NONE', #1772, #8255, #7192, .T. ) ;
#7859 = CARTESIAN_POINT ( 'NONE',  ( 0.8796985632579604752, -66.64547149457072805, 3.030887037049952326 ) ) ;
#7860 = CARTESIAN_POINT ( 'NONE',  ( -5.257311121191324155, -60.75452850542925631, 0.09995255151729526277 ) ) ;
#7861 = ORIENTED_EDGE ( 'NONE', *, *, #3011, .T. ) ;
#7862 = CARTESIAN_POINT ( 'NONE',  ( -1.719659006605374074, -63.15452850542925489, -4.969112962950016588 ) ) ;
#7863 = CARTESIAN_POINT ( 'NONE',  ( 6.686770931921479644, -85.39547149457074227, -2.072711028461788896 ) ) ;
#7864 =( NAMED_UNIT ( * ) PLANE_ANGLE_UNIT ( ) SI_UNIT ( $, .RADIAN. ) );
#7865 = ORIENTED_EDGE ( 'NONE', *, *, #6523, .T. ) ;
#7866 = CARTESIAN_POINT ( 'NONE',  ( -4.725907263620320542, -78.90452850542925489, 1.635492904037698647 ) ) ;
#7867 =( GEOMETRIC_REPRESENTATION_CONTEXT ( 3 ) GLOBAL_UNCERTAINTY_ASSIGNED_CONTEXT ( ( #6215 ) ) GLOBAL_UNIT_ASSIGNED_CONTEXT ( ( #4015, #815, #4680 ) ) REPRESENTATION_CONTEXT ( 'NONE', 'WORKASPACE' ) );
#7868 = LINE ( 'NONE', #2095, #8138 ) ;
#7869 = VECTOR ( 'NONE', #7347, 1000.000000000000000 ) ;
#7870 = CIRCLE ( 'NONE', #5307, 6.000000000000000000 ) ;
#7871 = DIRECTION ( 'NONE',  ( 1.000000000000000000, 0.000000000000000000, -0.000000000000000000 ) ) ;
#7872 = CARTESIAN_POINT ( 'NONE',  ( 5.257311121191341918, -76.24547149457073658, 0.09995255151718437925 ) ) ;
#7873 = CARTESIAN_POINT ( 'NONE',  ( -2.938187887435717016E-14, -97.00000000000001421, -3.999999999999997335 ) ) ;
#7874 = CARTESIAN_POINT ( 'NONE',  ( -3.154386672714792006, -59.74547149457073658, -0.09995255151720625064 ) ) ;
#7875 = CARTESIAN_POINT ( 'NONE',  ( -5.895805022753386027, -73.05452850542926058, 4.407101234057909878 ) ) ;
#7876 = DIRECTION ( 'NONE',  ( -0.000000000000000000, -0.000000000000000000, -1.000000000000000000 ) ) ;
#7877 = CARTESIAN_POINT ( 'NONE',  ( 4.725907263620372945, -76.09547149457074511, 1.635492904037598283 ) ) ;
#7878 = CARTESIAN_POINT ( 'NONE',  ( 54.99999999999999289, -30.00000000000000000, 7.499999999999992006 ) ) ;
#7879 = CARTESIAN_POINT ( 'NONE',  ( -4.784657899331189235, -87.60452850542925773, -1.454677039711773867 ) ) ;
#7880 = CARTESIAN_POINT ( 'NONE',  ( -6.686770931921506289, -66.60452850542924352, -2.072711028461647675 ) ) ;
#7881 = AXIS2_PLACEMENT_3D ( 'NONE', #5251, #912, #5970 ) ;
#7882 = CARTESIAN_POINT ( 'NONE',  ( -2.610703060766926153, -75.04547149457074795, 1.773238653441125745 ) ) ;
#7883 = EDGE_LOOP ( 'NONE', ( #6278, #5659, #6106, #5425, #658, #5171, #4368, #2413 ) ) ;
#7884 = DIRECTION ( 'NONE',  ( -0.000000000000000000, -0.000000000000000000, 1.000000000000000000 ) ) ;
#7885 = CARTESIAN_POINT ( 'NONE',  ( -3.015831842038213306, -93.30452850542926058, -3.989209796945429432 ) ) ;
#7886 = CARTESIAN_POINT ( 'NONE',  ( -4.194503406049316041, -85.05452850542926058, 3.171033256558100533 ) ) ;
#7887 = ORIENTED_EDGE ( 'NONE', *, *, #1617, .F. ) ;
#7888 = CARTESIAN_POINT ( 'NONE',  ( 1.529537955723690112, -74.85452850542925773, -5.030887037049978971 ) ) ;
#7889 = CARTESIAN_POINT ( 'NONE',  ( -0.8796985632579414904, -89.14547149457072805, -3.030887037049952326 ) ) ;
#7890 = CARTESIAN_POINT ( 'NONE',  ( 4.312004677471078296, -85.95452850542925205, 3.009306630940844496 ) ) ;
#7891 = CARTESIAN_POINT ( 'NONE',  ( 4.037591185471445243, -95.70452850542928047, -5.718994135553947977 ) ) ;
#7892 = CARTESIAN_POINT ( 'NONE',  ( 0.8796985632578979697, -68.85452850542924352, -3.030887037049972310 ) ) ;
#7893 = EDGE_CURVE ( 'NONE', #480, #200, #2012, .T. ) ;
#7894 = DIRECTION ( 'NONE',  ( 0.000000000000000000, 0.000000000000000000, 1.000000000000000000 ) ) ;
#7895 = PLANE ( 'NONE',  #397 ) ;
#7896 = CARTESIAN_POINT ( 'NONE',  ( 0.8796985632578991909, -77.85452850542925773, -3.030887037049972310 ) ) ;
#7897 = CARTESIAN_POINT ( 'NONE',  ( -4.037591185471421262, -91.20452850542925205, 5.718994135553947977 ) ) ;
#7898 = EDGE_CURVE ( 'NONE', #2910, #4617, #665, .T. ) ;
#7899 = DIRECTION ( 'NONE',  ( -0.000000000000000000, -0.000000000000000000, -1.000000000000000000 ) ) ;
#7900 = CARTESIAN_POINT ( 'NONE',  ( 6.686770931921479644, -85.39547149457074227, -2.072711028461788896 ) ) ;
#7901 = DIRECTION ( 'NONE',  ( -0.000000000000000000, -0.000000000000000000, -1.000000000000000000 ) ) ;
#7902 = CARTESIAN_POINT ( 'NONE',  ( 65.00000000000000000, -12.00000000000000711, 12.49999999999999822 ) ) ;
#7903 = CARTESIAN_POINT ( 'NONE',  ( -2.610703060766926598, -69.04547149457074795, 1.773238653441125745 ) ) ;
#7904 = CARTESIAN_POINT ( 'NONE',  ( -2.862020680886496304, -61.20452850542925205, 4.100960146804039752 ) ) ;
#7905 = ORIENTED_EDGE ( 'NONE', *, *, #6418, .T. ) ;
#7906 = CARTESIAN_POINT ( 'NONE',  ( 3.015831842038233290, -70.80452850542926058, 3.989209796945429432 ) ) ;
#7907 = CARTESIAN_POINT ( 'NONE',  ( 4.037591185471563371, -81.79547149457074795, 5.718994135553860936 ) ) ;
#7908 = ORIENTED_EDGE ( 'NONE', *, *, #1358, .F. ) ;
#7909 = CARTESIAN_POINT ( 'NONE',  ( 1.719659006605389839, -70.65452850542926910, 4.969112962950016588 ) ) ;
#7910 = CARTESIAN_POINT ( 'NONE',  ( -0.9662349396012467340, -27.25766265056033433, 4.500000000000000888 ) ) ;
#7911 = CONTEXT_DEPENDENT_SHAPE_REPRESENTATION ( #4005, #2325 ) ;
#7912 = CARTESIAN_POINT ( 'NONE',  ( -3.015831842038129817, -69.19547149457073942, 3.989209796945492048 ) ) ;
#7913 = DIRECTION ( 'NONE',  ( 0.000000000000000000, -1.000000000000000000, -1.734723475976807094E-16 ) ) ;
#7914 = CARTESIAN_POINT ( 'NONE',  ( -2.493201789345292241, -62.44547149457074653, -1.934965279058240561 ) ) ;
#7915 = CARTESIAN_POINT ( 'NONE',  ( -4.191402346623180009, -66.30452850542926058, -5.607243785695311900 ) ) ;
#7916 = DIRECTION ( 'NONE',  ( -1.000000000000000000, -0.000000000000000000, -0.000000000000000000 ) ) ;
#7917 =( NAMED_UNIT ( * ) SI_UNIT ( $, .STERADIAN. ) SOLID_ANGLE_UNIT ( ) );
#7918 = CARTESIAN_POINT ( 'NONE',  ( -1.719659006605371188, -84.15452850542925489, -4.969112962950016588 ) ) ;
#7919 = CARTESIAN_POINT ( 'NONE',  ( -7.360235569667858968, -69.75452850542926342, 0.09995255151731782806 ) ) ;
#7920 = CARTESIAN_POINT ( 'NONE',  ( 2.610703060766946138, -79.54547149457074795, -1.773238653441125523 ) ) ;
#7921 = ADVANCED_FACE ( 'NONE', ( #647 ), #5788, .F. ) ;
#7922 = AXIS2_PLACEMENT_3D ( 'NONE', #5877, #1419, #2733 ) ;
#7923 = ORIENTED_EDGE ( 'NONE', *, *, #4864, .T. ) ;
#7924 = DIRECTION ( 'NONE',  ( 0.000000000000000000, 1.000000000000000000, 2.168404344971010594E-16 ) ) ;
#7925 = LINE ( 'NONE', #7965, #1536 ) ;
#7926 = CARTESIAN_POINT ( 'NONE',  ( 1.719659006605390283, -73.65452850542924068, 4.969112962950016588 ) ) ;
#7927 = VERTEX_POINT ( 'NONE', #7740 ) ;
#7928 = CARTESIAN_POINT ( 'NONE',  ( -2.862020680886495416, -70.20452850542925205, 4.100960146804039752 ) ) ;
#7929 = CARTESIAN_POINT ( 'NONE',  ( -2.493201789345289132, -92.44547149457073942, -1.934965279058240561 ) ) ;
#7930 = CARTESIAN_POINT ( 'NONE',  ( -4.725907263620319654, -90.90452850542926910, 1.635492904037698647 ) ) ;
#7931 = CARTESIAN_POINT ( 'NONE',  ( 4.191402346623076980, -64.69547149457073942, -5.607243785695398941 ) ) ;
#7932 = CARTESIAN_POINT ( 'NONE',  ( -2.493201789345253161, -70.05452850542926058, 1.934965279058294518 ) ) ;
#7933 = EDGE_LOOP ( 'NONE', ( #6762, #4775, #6605, #1244 ) ) ;
#7934 = LINE ( 'NONE', #4714, #2947 ) ;
#7935 = CARTESIAN_POINT ( 'NONE',  ( -55.00000000000000000, -25.00000000000002132, 20.00000000000000000 ) ) ;
#7936 = CARTESIAN_POINT ( 'NONE',  ( -1.069819614139538411, -75.15452850542922647, -2.969112962950023249 ) ) ;
#7937 = CARTESIAN_POINT ( 'NONE',  ( 2.369498399071227279, -91.65452850542924068, 6.969112962950009482 ) ) ;
#7938 = AXIS2_PLACEMENT_3D ( 'NONE', #4207, #1013, #4671 ) ;
#7939 = CARTESIAN_POINT ( 'NONE',  ( -6.686770931921456551, -92.89547149457074227, 2.072711028461789784 ) ) ;
#7940 = CARTESIAN_POINT ( 'NONE',  ( -2.938187887435717016E-14, -97.00000000000001421, -3.999999999999997335 ) ) ;
#7941 = CARTESIAN_POINT ( 'NONE',  ( 65.00000000000000000, -12.00000000000000355, -12.50000000000000178 ) ) ;
#7942 = CARTESIAN_POINT ( 'NONE',  ( -2.882544866740859302, -65.89547149457074227, 0.8366430509619596778 ) ) ;
#7943 = VECTOR ( 'NONE', #1577, 1000.000000000000000 ) ;
#7944 = PLANE ( 'NONE',  #3892 ) ;
#7945 = SURFACE_STYLE_FILL_AREA ( #4769 ) ;
#7946 = ORIENTED_EDGE ( 'NONE', *, *, #1289, .T. ) ;
#7947 = CARTESIAN_POINT ( 'NONE',  ( -4.312004677471058756, -66.45452850542925205, -3.009306630940844052 ) ) ;
#7948 = CARTESIAN_POINT ( 'NONE',  ( -4.037591185471544719, -80.29547149457074795, -5.718994135553860936 ) ) ;
#7949 = VERTEX_POINT ( 'NONE', #5704 ) ;
#7950 = VECTOR ( 'NONE', #4673, 1000.000000000000000 ) ;
#7951 = CARTESIAN_POINT ( 'NONE',  ( 2.862020680886513180, -68.70452850542925205, -4.100960146804039752 ) ) ;
#7952 = DIRECTION ( 'NONE',  ( 0.000000000000000000, -0.000000000000000000, 1.000000000000000000 ) ) ;
#7953 = CARTESIAN_POINT ( 'NONE',  ( -4.312004677470993919, -72.04547149457074795, 3.009306630940933758 ) ) ;
#7954 = DIRECTION ( 'NONE',  ( 0.000000000000000000, -2.775557561562891351E-16, 1.000000000000000000 ) ) ;
#7955 = CARTESIAN_POINT ( 'NONE',  ( 5.257311121191343695, -97.24547149457075079, 0.09995255151718437925 ) ) ;
#7956 = CARTESIAN_POINT ( 'NONE',  ( 2.179377348189479591, -59.85452850542925773, -7.030887037049986077 ) ) ;
#7957 = ORIENTED_EDGE ( 'NONE', *, *, #374, .F. ) ;
#7958 = EDGE_CURVE ( 'NONE', #5889, #6843, #2688, .T. ) ;
#7959 = CARTESIAN_POINT ( 'NONE',  ( 65.00000000000000000, -7.999999999999996447, 12.49999999999999822 ) ) ;
#7960 = CARTESIAN_POINT ( 'NONE',  ( -4.312004677471056979, -81.45452850542923784, -3.009306630940844052 ) ) ;
#7961 = CARTESIAN_POINT ( 'NONE',  ( -4.191402346623180897, -63.30452850542926058, -5.607243785695311900 ) ) ;
#7962 = CARTESIAN_POINT ( 'NONE',  ( 2.610703060766944805, -73.54547149457074795, -1.773238653441125523 ) ) ;
#7963 = ORIENTED_EDGE ( 'NONE', *, *, #2458, .F. ) ;
#7964 = FACE_OUTER_BOUND ( 'NONE', #76, .T. ) ;
#7965 = CARTESIAN_POINT ( 'NONE',  ( -0.1932469879202498297, -30.15636746936407064, 4.500000000000000888 ) ) ;
#7966 = CARTESIAN_POINT ( 'NONE',  ( 4.784657899331209663, -77.10452850542925773, 1.454677039711774533 ) ) ;
#7967 = ORIENTED_EDGE ( 'NONE', *, *, #5515, .T. ) ;
#7968 = CARTESIAN_POINT ( 'NONE',  ( -4.784657899331190123, -72.60452850542925773, -1.454677039711773867 ) ) ;
#7969 = CARTESIAN_POINT ( 'NONE',  ( 1.686450176301638182, -93.79547149457076216, 2.482926158054096000 ) ) ;
#7970 = CARTESIAN_POINT ( 'NONE',  ( -1.529537955723774489, -95.14547149457074227, -5.030887037049945221 ) ) ;
#7971 = CARTESIAN_POINT ( 'NONE',  ( 4.312004677471075631, -76.95452850542923784, 3.009306630940844496 ) ) ;
#7972 = CARTESIAN_POINT ( 'NONE',  ( 7.360235569667880284, -89.25452850542926342, -0.09995255151731691212 ) ) ;
#7973 = CARTESIAN_POINT ( 'NONE',  ( -1.686450176301566906, -67.20452850542925205, 2.482926158054133303 ) ) ;
#7974 = ORIENTED_EDGE ( 'NONE', *, *, #4086, .T. ) ;
#7975 = CARTESIAN_POINT ( 'NONE',  ( 1.500000000000001998, -26.99999999999998934, 0.000000000000000000 ) ) ;
#7976 = LINE ( 'NONE', #5989, #944 ) ;
#7977 = CARTESIAN_POINT ( 'NONE',  ( -1.840261337453251933, -75.30452850542926058, -2.371175808195547852 ) ) ;
#7978 = CARTESIAN_POINT ( 'NONE',  ( -2.179377348189459607, -91.35452850542925773, 7.030887037049988741 ) ) ;
#7979 = CARTESIAN_POINT ( 'NONE',  ( 2.179377348189630581, -87.64547149457075648, 7.030887037049939003 ) ) ;
#7980 = DIRECTION ( 'NONE',  ( 0.000000000000000000, 0.000000000000000000, -1.000000000000000000 ) ) ;
#7981 = CARTESIAN_POINT ( 'NONE',  ( 43.50000000000000711, -14.99999999999999467, -12.50000000000000178 ) ) ;
#7982 = CARTESIAN_POINT ( 'NONE',  ( -3.154386672714790674, -71.74547149457075079, -0.09995255151720625064 ) ) ;
#7983 = PRODUCT_DEFINITION_CONTEXT ( 'detailed design', #7343, 'design' ) ;
#7984 = ORIENTED_EDGE ( 'NONE', *, *, #6263, .T. ) ;
#7985 = VECTOR ( 'NONE', #2464, 1000.000000000000000 ) ;
#7986 = CARTESIAN_POINT ( 'NONE',  ( -0.09506052544084148126, -66.00452850542926342, -4.999999999999997335 ) ) ;
#7987 = CARTESIAN_POINT ( 'NONE',  ( -7.360235569667858080, -83.74547149457075079, -0.09995255151716124498 ) ) ;
#7988 = VERTEX_POINT ( 'NONE', #5245 ) ;
#7989 = CARTESIAN_POINT ( 'NONE',  ( 3.015831842038148913, -76.69547149457075363, -3.989209796945492048 ) ) ;
#7990 = CARTESIAN_POINT ( 'NONE',  ( -1.719659006605373630, -66.15452850542926910, -4.969112962950016588 ) ) ;
#7991 = DIRECTION ( 'NONE',  ( -0.000000000000000000, 0.000000000000000000, 1.000000000000000000 ) ) ;
#7992 = PRODUCT_RELATED_PRODUCT_CATEGORY ( 'part', '', ( #4128 ) ) ;
#7993 = CARTESIAN_POINT ( 'NONE',  ( -4.194503406049384431, -71.44547149457075363, -3.171033256558012159 ) ) ;
#7994 = CARTESIAN_POINT ( 'NONE',  ( 43.50000000000000711, -14.99999999999999467, 4.500000000000000888 ) ) ;
#7995 = CARTESIAN_POINT ( 'NONE',  ( -1.529537955723774489, -95.14547149457074227, -5.030887037049945221 ) ) ;
#7996 = VECTOR ( 'NONE', #7115, 1000.000000000000000 ) ;
#7997 = CARTESIAN_POINT ( 'NONE',  ( 6.013306294175167821, -61.95452850542925916, 4.245374608440616093 ) ) ;
#7998 = EDGE_LOOP ( 'NONE', ( #1827, #858, #3814, #641, #519, #4665, #6219, #5594 ) ) ;
#7999 = CIRCLE ( 'NONE', #7585, 6.000000000000000000 ) ;
#8000 = AXIS2_PLACEMENT_3D ( 'NONE', #393, #6087, #6717 ) ;
#8001 = VECTOR ( 'NONE', #784, 1000.000000000000000 ) ;
#8002 = PRESENTATION_LAYER_ASSIGNMENT (  '', '', ( #6914 ) ) ;
#8003 = ORIENTED_EDGE ( 'NONE', *, *, #2532, .T. ) ;
#8004 = LINE ( 'NONE', #2900, #1331 ) ;
#8005 = CARTESIAN_POINT ( 'NONE',  ( -5.257311121191323267, -84.75452850542923500, 0.09995255151729526277 ) ) ;
#8006 = CARTESIAN_POINT ( 'NONE',  ( -3.015831842038215083, -75.30452850542926058, -3.989209796945429432 ) ) ;
#8007 = ORIENTED_EDGE ( 'NONE', *, *, #8144, .F. ) ;
#8008 = CARTESIAN_POINT ( 'NONE',  ( -3.015831842038215527, -72.30452850542926058, -3.989209796945429432 ) ) ;
#8009 = CARTESIAN_POINT ( 'NONE',  ( 1.840261337453220847, -82.69547149457073942, -2.371175808195584267 ) ) ;
#8010 = VECTOR ( 'NONE', #8161, 1000.000000000000000 ) ;
#8011 = CARTESIAN_POINT ( 'NONE',  ( 4.784657899331180353, -97.39547149457074227, -1.454677039711874009 ) ) ;
#8012 = CARTESIAN_POINT ( 'NONE',  ( 4.194503406049338246, -80.55452850542926058, -3.171033256558100089 ) ) ;
#8013 = CARTESIAN_POINT ( 'NONE',  ( -6.628020296210619833, -90.90452850542926910, 2.253526892787613978 ) ) ;
#8014 = EDGE_CURVE ( 'NONE', #4198, #4811, #6592, .T. ) ;
#8015 = CARTESIAN_POINT ( 'NONE',  ( -0.8796985632578812053, -61.35452850542925773, 3.030887037049973198 ) ) ;
#8016 = ORIENTED_EDGE ( 'NONE', *, *, #2821, .F. ) ;
#8017 = DIRECTION ( 'NONE',  ( -1.000000000000000000, -9.251858538542971581E-17, 0.000000000000000000 ) ) ;
#8018 = VERTEX_POINT ( 'NONE', #1929 ) ;
#8019 = LINE ( 'NONE', #5352, #1623 ) ;
#8020 = CARTESIAN_POINT ( 'NONE',  ( 1.069819614139556840, -73.65452850542925489, 2.969112962950023249 ) ) ;
#8021 = CARTESIAN_POINT ( 'NONE',  ( -7.360235569667858080, -84.75452850542926342, 0.09995255151731782806 ) ) ;
#8022 = CARTESIAN_POINT ( 'NONE',  ( 6.628020296210689111, -82.09547149457075932, 2.253526892787472757 ) ) ;
#8023 = LINE ( 'NONE', #2250, #7510 ) ;
#8024 = CARTESIAN_POINT ( 'NONE',  ( -1.529537955723774711, -95.14547149457074227, -5.030887037049945221 ) ) ;
#8025 = CARTESIAN_POINT ( 'NONE',  ( -2.882544866740876621, -81.60452850542927195, -0.8366430509618996147 ) ) ;
#8026 = EDGE_CURVE ( 'NONE', #5238, #6672, #3820, .T. ) ;
#8027 = DIRECTION ( 'NONE',  ( -9.251858538542972814E-17, 1.000000000000000000, 0.000000000000000000 ) ) ;
#8028 = VERTEX_POINT ( 'NONE', #7697 ) ;
#8029 = CARTESIAN_POINT ( 'NONE',  ( -5.999999999999993783, -47.00000000000000000, 2.500000000000000888 ) ) ;
#8030 = CARTESIAN_POINT ( 'NONE',  ( -3.015831842038215527, -72.30452850542926058, -3.989209796945429432 ) ) ;
#8031 = CARTESIAN_POINT ( 'NONE',  ( -6.013306294175058575, -84.04547149457074795, 4.245374608440741326 ) ) ;
#8032 = ORIENTED_EDGE ( 'NONE', *, *, #8112, .T. ) ;
#8033 = CARTESIAN_POINT ( 'NONE',  ( 2.862020680886599333, -75.79547149457074795, 4.100960146803977580 ) ) ;
#8034 = CARTESIAN_POINT ( 'NONE',  ( 4.312004677471011682, -73.54547149457073374, -3.009306630940933314 ) ) ;
#8035 = CARTESIAN_POINT ( 'NONE',  ( -4.312004677471060532, -63.45452850542926626, -3.009306630940844052 ) ) ;
#8036 = CARTESIAN_POINT ( 'NONE',  ( 55.00000000000002132, -99.99999999999998579, 20.00000000000000000 ) ) ;
#8037 = CARTESIAN_POINT ( 'NONE',  ( 0.09506052544075412059, -67.99547149457075079, -4.999999999999997335 ) ) ;
#8038 = CARTESIAN_POINT ( 'NONE',  ( 0.3811618011801478634, -97.00000000000001421, -4.000000000000000888 ) ) ;
#8039 = CARTESIAN_POINT ( 'NONE',  ( 5.895805022753402902, -59.55452850542924637, -4.407101234057908989 ) ) ;
#8040 = VERTEX_POINT ( 'NONE', #3985 ) ;
#8041 = DIRECTION ( 'NONE',  ( 0.000000000000000000, 0.000000000000000000, 1.000000000000000000 ) ) ;
#8042 = PRODUCT ( 'return spring', 'return spring', '', ( #6346 ) ) ;
#8043 = ORIENTED_EDGE ( 'NONE', *, *, #6924, .F. ) ;
#8044 = DIRECTION ( 'NONE',  ( 0.000000000000000000, -1.000000000000000000, 0.000000000000000000 ) ) ;
#8045 = CARTESIAN_POINT ( 'NONE',  ( 2.862020680886514956, -83.70452850542925205, -4.100960146804039752 ) ) ;
#8046 = CARTESIAN_POINT ( 'NONE',  ( -4.312004677471056979, -81.45452850542923784, -3.009306630940844052 ) ) ;
#8047 = EDGE_LOOP ( 'NONE', ( #7075, #7551, #6093, #6437 ) ) ;
#8048 = CARTESIAN_POINT ( 'NONE',  ( -2.862020680886495416, -67.20452850542925205, 4.100960146804039752 ) ) ;
#8049 = CARTESIAN_POINT ( 'NONE',  ( 2.493201789345310004, -78.94547149457073942, 1.934965279058241006 ) ) ;
#8050 = CARTESIAN_POINT ( 'NONE',  ( -3.154386672714792006, -59.74547149457073658, -0.09995255151720625064 ) ) ;
#8051 = CARTESIAN_POINT ( 'NONE',  ( 3.015831842038233734, -73.80452850542926058, 3.989209796945429432 ) ) ;
#8052 = CARTESIAN_POINT ( 'NONE',  ( 6.013306294175171374, -88.95452850542925205, 4.245374608440616093 ) ) ;
#8053 = AXIS2_PLACEMENT_3D ( 'NONE', #2675, #3973, #6499 ) ;
#8054 = CARTESIAN_POINT ( 'NONE',  ( -2.610703060766967454, -57.45452850542925916, -1.773238653441072232 ) ) ;
#8055 = ORIENTED_EDGE ( 'NONE', *, *, #2178, .T. ) ;
#8056 = DIRECTION ( 'NONE',  ( -1.000000000000000000, 0.000000000000000000, 0.000000000000000000 ) ) ;
#8057 = ORIENTED_EDGE ( 'NONE', *, *, #3535, .T. ) ;
#8058 = CARTESIAN_POINT ( 'NONE',  ( -4.056271377811393464E-14, -97.00000000000000000, -4.999999999999996447 ) ) ;
#8059 = CARTESIAN_POINT ( 'NONE',  ( -2.882544866740878842, -66.60452850542924352, -0.8366430509618996147 ) ) ;
#8060 = CARTESIAN_POINT ( 'NONE',  ( -2.179377348189610597, -77.14547149457074227, -7.030887037049939003 ) ) ;
#8061 = CARTESIAN_POINT ( 'NONE',  ( -47.50000000000000711, -51.00000000000000711, -12.50000000000001954 ) ) ;
#8062 = CARTESIAN_POINT ( 'NONE',  ( 4.312004677471013459, -94.54547149457073374, -3.009306630940932425 ) ) ;
#8063 = CARTESIAN_POINT ( 'NONE',  ( -0.09506052544081858291, -81.00452850542926342, -2.999999999999997780 ) ) ;
#8064 = EDGE_CURVE ( 'NONE', #1590, #1139, #1270, .T. ) ;
#8065 = PRODUCT_DEFINITION_CONTEXT ( 'detailed design', #1421, 'design' ) ;
#8066 = FACE_OUTER_BOUND ( 'NONE', #5657, .T. ) ;
#8067 = EDGE_LOOP ( 'NONE', ( #6548, #1003 ) ) ;
#8068 = FACE_OUTER_BOUND ( 'NONE', #5822, .T. ) ;
#8069 = CARTESIAN_POINT ( 'NONE',  ( -0.09506052544084261924, -57.00452850542924921, -4.999999999999997335 ) ) ;
#8070 = VECTOR ( 'NONE', #5988, 1000.000000000000000 ) ;
#8071 = CARTESIAN_POINT ( 'NONE',  ( -0.09506052544071530441, -66.49547149457075079, 6.999999999999997335 ) ) ;
#8072 = ORIENTED_EDGE ( 'NONE', *, *, #6344, .T. ) ;
#8073 = CARTESIAN_POINT ( 'NONE',  ( -4.784657899331159037, -71.89547149457074227, 1.454677039711874675 ) ) ;
#8074 = CARTESIAN_POINT ( 'NONE',  ( 1.719659006605285034, -70.84547149457074511, -4.969112962950050338 ) ) ;
#8075 = CARTESIAN_POINT ( 'NONE',  ( -1.719659006605373408, -69.15452850542924068, -4.969112962950016588 ) ) ;
#8076 = DIRECTION ( 'NONE',  ( 1.387778780781445478E-15, -1.000000000000000000, 0.000000000000000000 ) ) ;
#8077 = AXIS2_PLACEMENT_3D ( 'NONE', #2038, #1994, #7850 ) ;
#8078 = AXIS2_PLACEMENT_3D ( 'NONE', #7657, #3317, #5202 ) ;
#8079 = CARTESIAN_POINT ( 'NONE',  ( 1.719659006605284590, -67.84547149457070248, -4.969112962950050338 ) ) ;
#8080 = CARTESIAN_POINT ( 'NONE',  ( -2.369498399071207739, -60.15452850542926200, -6.969112962950009482 ) ) ;
#8081 = ORIENTED_EDGE ( 'NONE', *, *, #4273, .T. ) ;
#8082 = DIRECTION ( 'NONE',  ( 1.000000000000000000, 0.000000000000000000, 0.000000000000000000 ) ) ;
#8083 = COLOUR_RGB ( '', 0.66274510, 0.83137255, 0.94901961) ;
#8084 = EDGE_CURVE ( 'NONE', #3622, #3916, #148, .T. ) ;
#8085 = VERTEX_POINT ( 'NONE', #4652 ) ;
#8086 = LINE ( 'NONE', #3651, #5433 ) ;
#8087 = CARTESIAN_POINT ( 'NONE',  ( 0.09506052544086160405, -88.50452850542924921, 4.999999999999997335 ) ) ;
#8088 = CARTESIAN_POINT ( 'NONE',  ( -1.719659006605371854, -78.15452850542925489, -4.969112962950016588 ) ) ;
#8089 = CARTESIAN_POINT ( 'NONE',  ( -4.194503406049320482, -61.05452850542925347, 3.171033256558101865 ) ) ;
#8090 = CARTESIAN_POINT ( 'NONE',  ( 1.069819614139494446, -76.84547149457073090, -2.969112962950042789 ) ) ;
#8091 = MECHANICAL_DESIGN_GEOMETRIC_PRESENTATION_REPRESENTATION (  '', ( #4854 ), #6602 ) ;
#8092 = CARTESIAN_POINT ( 'NONE',  ( 4.312004677471013459, -94.54547149457071953, -3.009306630940933314 ) ) ;
#8093 = CARTESIAN_POINT ( 'NONE',  ( -1.719659006605373408, -69.15452850542924068, -4.969112962950016588 ) ) ;
#8094 = CARTESIAN_POINT ( 'NONE',  ( -6.013306294175150946, -84.45452850542925205, -4.245374608440613429 ) ) ;
#8095 = CARTESIAN_POINT ( 'NONE',  ( 0.09506052544083691547, -61.50452850542925631, 2.999999999999997780 ) ) ;
#8096 = APPLICATION_PROTOCOL_DEFINITION ( 'draft international standard', 'automotive_design', 1998, #7343 ) ;
#8097 = EDGE_CURVE ( 'NONE', #4811, #5032, #7233, .T. ) ;
#8098 = ORIENTED_EDGE ( 'NONE', *, *, #3692, .T. ) ;
#8099 = CARTESIAN_POINT ( 'NONE',  ( 0.000000000000000000, 0.000000000000000000, 20.00000000000000000 ) ) ;
#8100 = ORIENTED_EDGE ( 'NONE', *, *, #5597, .F. ) ;
#8101 = CARTESIAN_POINT ( 'NONE',  ( 0.000000000000000000, -9.999999999999994671, -34.24264068711928388 ) ) ;
#8102 = CARTESIAN_POINT ( 'NONE',  ( 1.686450176301584225, -68.70452850542925205, -2.482926158054133303 ) ) ;
#8103 = CARTESIAN_POINT ( 'NONE',  ( -2.179377348189610597, -80.14547149457074227, -7.030887037049939003 ) ) ;
#8104 = CARTESIAN_POINT ( 'NONE',  ( -4.784657899331189235, -90.60452850542925773, -1.454677039711773867 ) ) ;
#8105 = CARTESIAN_POINT ( 'NONE',  ( 1.719659006605287921, -94.84547149457074511, -4.969112962950050338 ) ) ;
#8106 = CARTESIAN_POINT ( 'NONE',  ( 1.069819614139558173, -85.65452850542926910, 2.969112962950023249 ) ) ;
#8107 = ORIENTED_EDGE ( 'NONE', *, *, #6258, .F. ) ;
#8108 = CARTESIAN_POINT ( 'NONE',  ( 95.11234224026316042, -46.99999999999999289, -20.00000000000000000 ) ) ;
#8109 = CARTESIAN_POINT ( 'NONE',  ( 2.823794231030042567, -95.40452850542926910, -1.017458915287783316 ) ) ;
#8110 = CARTESIAN_POINT ( 'NONE',  ( -2.369498399071057637, -72.34547149457073090, 6.969112962950058332 ) ) ;
#8111 = CARTESIAN_POINT ( 'NONE',  ( 4.430245668755248722, -96.99999999999997158, 2.549500813230844543 ) ) ;
#8112 = EDGE_CURVE ( 'NONE', #6779, #4647, #5380, .T. ) ;
#8113 = PRODUCT_DEFINITION_SHAPE ( 'NONE', 'NONE',  #8344 ) ;
#8114 = CARTESIAN_POINT ( 'NONE',  ( 4.784657899331176800, -73.39547149457074227, -1.454677039711874009 ) ) ;
#8115 = CARTESIAN_POINT ( 'NONE',  ( 5.257311121191341918, -67.24547149457075079, 0.09995255151718437925 ) ) ;
#8116 = CARTESIAN_POINT ( 'NONE',  ( 4.312004677471074743, -67.95452850542922363, 3.009306630940844496 ) ) ;
#8117 = LINE ( 'NONE', #312, #2218 ) ;
#8118 = CIRCLE ( 'NONE', #4070, 1.500000000000001332 ) ;
#8119 = CARTESIAN_POINT ( 'NONE',  ( 2.862020680886598001, -63.79547149457074084, 4.100960146803977580 ) ) ;
#8120 = CARTESIAN_POINT ( 'NONE',  ( 0.000000000000000000, 0.000000000000000000, 0.000000000000000000 ) ) ;
#8121 = CARTESIAN_POINT ( 'NONE',  ( -1.529537955723667908, -94.35452850542922931, 5.030887037049979860 ) ) ;
#8122 = VERTEX_POINT ( 'NONE', #7994 ) ;
#8123 = DIRECTION ( 'NONE',  ( -0.000000000000000000, -0.000000000000000000, -1.000000000000000000 ) ) ;
#8124 = VERTEX_POINT ( 'NONE', #2099 ) ;
#8125 = CARTESIAN_POINT ( 'NONE',  ( -3.989863994746656317E-14, -97.00000000000000000, -4.999999999999997335 ) ) ;
#8126 = CARTESIAN_POINT ( 'NONE',  ( -4.784657899331189235, -90.60452850542925773, -1.454677039711773867 ) ) ;
#8127 = VECTOR ( 'NONE', #5582, 1000.000000000000000 ) ;
#8128 = CARTESIAN_POINT ( 'NONE',  ( -2.862020680886578905, -92.29547149457074795, -4.100960146803977580 ) ) ;
#8129 = CARTESIAN_POINT ( 'NONE',  ( -4.312004677471058756, -66.45452850542925205, -3.009306630940843608 ) ) ;
#8130 = CARTESIAN_POINT ( 'NONE',  ( -1.069819614139474240, -81.34547149457074511, 2.969112962950044121 ) ) ;
#8131 = CARTESIAN_POINT ( 'NONE',  ( -3.015831842038128041, -84.19547149457073942, 3.989209796945492048 ) ) ;
#8132 = CARTESIAN_POINT ( 'NONE',  ( -4.194503406049319594, -67.05452850542926058, 3.171033256558100533 ) ) ;
#8133 = CARTESIAN_POINT ( 'NONE',  ( 7.360235569667878508, -83.25452850542926342, -0.09995255151731691212 ) ) ;
#8134 = CARTESIAN_POINT ( 'NONE',  ( -1.069819614139472019, -96.34547149457074511, 2.969112962950044121 ) ) ;
#8135 = APPLICATION_PROTOCOL_DEFINITION ( 'draft international standard', 'automotive_design', 1998, #5879 ) ;
#8136 = ORIENTED_EDGE ( 'NONE', *, *, #3601, .T. ) ;
#8137 = CARTESIAN_POINT ( 'NONE',  ( 80.00000000000000000, -9.999999999999994671, 0.000000000000000000 ) ) ;
#8138 = VECTOR ( 'NONE', #2136, 1000.000000000000000 ) ;
#8139 = ORIENTED_EDGE ( 'NONE', *, *, #520, .T. ) ;
#8140 = CARTESIAN_POINT ( 'NONE',  ( 4.784657899331212327, -95.10452850542925773, 1.454677039711774533 ) ) ;
#8141 = CARTESIAN_POINT ( 'NONE',  ( 0.09506052544083806732, -70.50452850542926342, 2.999999999999997780 ) ) ;
#8142 = CARTESIAN_POINT ( 'NONE',  ( -0.09506052544071341703, -81.49547149457075079, 6.999999999999997335 ) ) ;
#8143 = CARTESIAN_POINT ( 'NONE',  ( -5.257311121191321490, -93.75452850542926342, 0.09995255151729526277 ) ) ;
#8144 = EDGE_CURVE ( 'NONE', #97, #1554, #1456, .T. ) ;
#8145 = CARTESIAN_POINT ( 'NONE',  ( -2.823794231030019475, -87.90452850542926910, 1.017458915287783316 ) ) ;
#8146 = PRODUCT_DEFINITION_SHAPE ( 'NONE', 'NONE',  #8349 ) ;
#8147 = CARTESIAN_POINT ( 'NONE',  ( 1.500000000000002442, -27.00000000000000000, -2.499999999999999556 ) ) ;
#8148 = ORIENTED_EDGE ( 'NONE', *, *, #5640, .T. ) ;
#8149 = ADVANCED_FACE ( 'NONE', ( #4822 ), #6597, .T. ) ;
#8150 = CARTESIAN_POINT ( 'NONE',  ( 3.154386672714811102, -95.25452850542926342, -0.09995255151727241993 ) ) ;
#8151 = CARTESIAN_POINT ( 'NONE',  ( 0.09506052544073312349, -67.99547149457075079, -6.999999999999997335 ) ) ;
#8152 = CARTESIAN_POINT ( 'NONE',  ( 2.712844317851120124, -96.99999999999997158, -5.329299858373291343 ) ) ;
#8153 = CARTESIAN_POINT ( 'NONE',  ( -1.719659006605265272, -78.34547149457074511, 4.969112962950051227 ) ) ;
#8154 = CARTESIAN_POINT ( 'NONE',  ( -0.09506052544073578803, -72.49547149457075079, 4.999999999999997335 ) ) ;
#8155 = CARTESIAN_POINT ( 'NONE',  ( -1.529537955723672349, -58.35452850542924352, 5.030887037049979860 ) ) ;
#8156 = DIRECTION ( 'NONE',  ( -0.000000000000000000, -0.000000000000000000, -1.000000000000000000 ) ) ;
#8157 = CARTESIAN_POINT ( 'NONE',  ( 4.725907263620340082, -71.40452850542925489, -1.635492904037697981 ) ) ;
#8158 = CARTESIAN_POINT ( 'NONE',  ( -5.257311121191324155, -62.74547149457075079, -0.09995255151718371311 ) ) ;
#8159 = VERTEX_POINT ( 'NONE', #6677 ) ;
#8160 = UNCERTAINTY_MEASURE_WITH_UNIT (LENGTH_MEASURE( 1.000000000000000082E-05 ), #4857, 'distance_accuracy_value', 'NONE');
#8161 = DIRECTION ( 'NONE',  ( 1.000000000000000000, 0.000000000000000000, 0.000000000000000000 ) ) ;
#8162 = ORIENTED_EDGE ( 'NONE', *, *, #866, .F. ) ;
#8163 = FACE_OUTER_BOUND ( 'NONE', #5696, .T. ) ;
#8164 = CARTESIAN_POINT ( 'NONE',  ( -5.257311121191322378, -87.75452850542922079, 0.09995255151729526277 ) ) ;
#8165 = CARTESIAN_POINT ( 'NONE',  ( -1.529537955723776044, -86.14547149457074227, -5.030887037049945221 ) ) ;
#8166 = CARTESIAN_POINT ( 'NONE',  ( -1.529537955723672127, -61.35452850542925773, 5.030887037049979860 ) ) ;
#8167 = CARTESIAN_POINT ( 'NONE',  ( -0.09506052544075634103, -78.49547149457075079, 2.999999999999997780 ) ) ;
#8168 = CARTESIAN_POINT ( 'NONE',  ( -6.686770931921506289, -75.60452850542924352, -2.072711028461647675 ) ) ;
#8169 = CARTESIAN_POINT ( 'NONE',  ( 0.09506052544075714594, -91.99547149457073658, -4.999999999999997335 ) ) ;
#8170 = CARTESIAN_POINT ( 'NONE',  ( -4.194503406049320482, -64.05452850542926058, 3.171033256558100533 ) ) ;
#8171 = CARTESIAN_POINT ( 'NONE',  ( -6.013306294175150946, -81.45452850542925205, -4.245374608440613429 ) ) ;
#8172 = CARTESIAN_POINT ( 'NONE',  ( 2.493201789345312669, -96.94547149457073942, 1.934965279058241006 ) ) ;
#8173 = EDGE_CURVE ( 'NONE', #2454, #8018, #5964, .T. ) ;
#8174 = ORIENTED_EDGE ( 'NONE', *, *, #2393, .F. ) ;
#8175 = DIRECTION ( 'NONE',  ( 1.000000000000000000, -0.000000000000000000, -0.000000000000000000 ) ) ;
#8176 = ORIENTED_EDGE ( 'NONE', *, *, #2178, .F. ) ;
#8177 = CARTESIAN_POINT ( 'NONE',  ( -2.862020680886492308, -91.20452850542926626, 4.100960146804039752 ) ) ;
#8178 = CARTESIAN_POINT ( 'NONE',  ( 0.09506052544083729017, -64.50452850542926342, 2.999999999999997780 ) ) ;
#8179 = CARTESIAN_POINT ( 'NONE',  ( -5.895805022753386915, -61.05452850542925347, 4.407101234057909878 ) ) ;
#8180 = CARTESIAN_POINT ( 'NONE',  ( 7.360235569667877620, -79.24547149457073658, 0.09995255151716216091 ) ) ;
#8181 = DIRECTION ( 'NONE',  ( 1.000000000000000000, 0.000000000000000000, 0.000000000000000000 ) ) ;
#8182 = CARTESIAN_POINT ( 'NONE',  ( -1.529537955723776488, -83.14547149457072805, -5.030887037049945221 ) ) ;
#8183 = CARTESIAN_POINT ( 'NONE',  ( 2.823794231030041235, -83.40452850542925489, -1.017458915287783316 ) ) ;
#8184 = FILL_AREA_STYLE ('',( #7511 ) ) ;
#8185 = EDGE_LOOP ( 'NONE', ( #7842, #6480 ) ) ;
#8186 = SURFACE_SIDE_STYLE ('',( #4417 ) ) ;
#8187 = CARTESIAN_POINT ( 'NONE',  ( -1.840261337453249491, -93.30452850542926058, -2.371175808195547852 ) ) ;
#8188 = CARTESIAN_POINT ( 'NONE',  ( 2.179377348189629249, -72.64547149457072805, 7.030887037049939003 ) ) ;
#8189 = CARTESIAN_POINT ( 'NONE',  ( 4.742539934031843707, -96.99999999999982947, 2.318475365005189026 ) ) ;
#8190 = CARTESIAN_POINT ( 'NONE',  ( -4.725907263620354293, -68.59547149457073090, -1.635492904037597617 ) ) ;
#8191 = CARTESIAN_POINT ( 'NONE',  ( 0.09506052544075374588, -64.99547149457075079, -4.999999999999997335 ) ) ;
#8192 = CARTESIAN_POINT ( 'NONE',  ( 1.686450176301588000, -95.70452850542928047, -2.482926158054133303 ) ) ;
#8193 = CARTESIAN_POINT ( 'NONE',  ( 80.00000000000000000, -9.999999999999994671, 10.50000000000000533 ) ) ;
#8194 = CARTESIAN_POINT ( 'NONE',  ( 4.725907263620340082, -65.40452850542925489, -1.635492904037697981 ) ) ;
#8195 = CARTESIAN_POINT ( 'NONE',  ( 4.191402346623081421, -97.69547149457076785, -5.607243785695398941 ) ) ;
#8196 = ORIENTED_EDGE ( 'NONE', *, *, #8064, .F. ) ;
#8197 = CIRCLE ( 'NONE', #6309, 1.500000000000001776 ) ;
#8198 = LINE ( 'NONE', #2430, #6789 ) ;
#8199 = PRODUCT_DEFINITION_FORMATION_WITH_SPECIFIED_SOURCE ( 'ANY', '', #1716, .NOT_KNOWN. ) ;
#8200 = ORIENTED_EDGE ( 'NONE', *, *, #3935, .F. ) ;
#8201 = DIRECTION ( 'NONE',  ( 0.000000000000000000, -0.7071067811865484609, -0.7071067811865465735 ) ) ;
#8202 = CARTESIAN_POINT ( 'NONE',  ( -2.862020680886494084, -79.20452850542925205, 4.100960146804039752 ) ) ;
#8203 = CARTESIAN_POINT ( 'NONE',  ( -4.312004677470991254, -93.04547149457074795, 3.009306630940933758 ) ) ;
#8204 = ADVANCED_FACE ( 'NONE', ( #192 ), #2771, .F. ) ;
#8205 = CARTESIAN_POINT ( 'NONE',  ( 1.529537955723688336, -59.85452850542925063, -5.030887037049978971 ) ) ;
#8206 = CARTESIAN_POINT ( 'NONE',  ( 0.09506052544077554789, -70.99547149457075079, -2.999999999999997780 ) ) ;
#8207 = CARTESIAN_POINT ( 'NONE',  ( 6.013306294175169597, -79.95452850542925205, 4.245374608440616093 ) ) ;
#8208 = CARTESIAN_POINT ( 'NONE',  ( -4.194503406049382654, -92.44547149457073942, -3.171033256558012159 ) ) ;
#8209 = CARTESIAN_POINT ( 'NONE',  ( 4.312004677471073855, -64.95452850542926626, 3.009306630940844496 ) ) ;
#8210 = AXIS2_PLACEMENT_3D ( 'NONE', #2894, #2852, #7913 ) ;
#8211 = CARTESIAN_POINT ( 'NONE',  ( 6.628020296210641149, -74.40452850542925489, -2.253526892787612645 ) ) ;
#8212 = CARTESIAN_POINT ( 'NONE',  ( -1.840261337453198864, -87.19547149457073942, 2.371175808195584267 ) ) ;
#8213 = ORIENTED_EDGE ( 'NONE', *, *, #3178, .T. ) ;
#8214 = DIRECTION ( 'NONE',  ( 0.000000000000000000, -0.7071067811865483499, -0.7071067811865465735 ) ) ;
#8215 = LINE ( 'NONE', #7752, #3143 ) ;
#8216 = COLOUR_RGB ( '', 0.09019608, 0.27058824, 0.51372549) ;
#8217 = ORIENTED_EDGE ( 'NONE', *, *, #1238, .F. ) ;
#8218 = CARTESIAN_POINT ( 'NONE',  ( -4.725907263620319654, -87.90452850542926910, 1.635492904037698647 ) ) ;
#8219 = CARTESIAN_POINT ( 'NONE',  ( -1.686450176301566684, -70.20452850542925205, 2.482926158054133303 ) ) ;
#8220 = CARTESIAN_POINT ( 'NONE',  ( -6.013306294175155386, -57.45452850542925916, -4.245374608440613429 ) ) ;
#8221 = CARTESIAN_POINT ( 'NONE',  ( -6.013306294175061240, -69.04547149457074795, 4.245374608440741326 ) ) ;
#8222 = CARTESIAN_POINT ( 'NONE',  ( 4.725907263620373833, -82.09547149457074511, 1.635492904037598283 ) ) ;
#8223 = CARTESIAN_POINT ( 'NONE',  ( 2.610703060766983885, -79.95452850542925205, 1.773238653441072232 ) ) ;
#8224 = DIRECTION ( 'NONE',  ( 1.000000000000000000, 0.000000000000000000, 0.000000000000000000 ) ) ;
#8225 = ORIENTED_EDGE ( 'NONE', *, *, #6508, .F. ) ;
#8226 = CARTESIAN_POINT ( 'NONE',  ( -4.784657899331192787, -57.60452850542925773, -1.454677039711773867 ) ) ;
#8227 = CARTESIAN_POINT ( 'NONE',  ( 4.037591185471561595, -69.79547149457074795, 5.718994135553860936 ) ) ;
#8228 = CARTESIAN_POINT ( 'NONE',  ( 0.000000000000000000, 0.000000000000000000, 0.000000000000000000 ) ) ;
#8229 = CARTESIAN_POINT ( 'NONE',  ( 4.546448683094512333, -96.99999999999961631, 2.488164940520385837 ) ) ;
#8230 = CARTESIAN_POINT ( 'NONE',  ( 4.194503406049400418, -66.94547149457075363, 3.171033256558012159 ) ) ;
#8231 = CARTESIAN_POINT ( 'NONE',  ( -0.09506052544073692601, -63.49547149457074369, 4.999999999999997335 ) ) ;
#8232 = CARTESIAN_POINT ( 'NONE',  ( -2.493201789345250052, -94.05452850542926058, 1.934965279058294518 ) ) ;
#8233 = DIRECTION ( 'NONE',  ( 1.000000000000000000, 0.000000000000000000, 0.000000000000000000 ) ) ;
#8234 = CARTESIAN_POINT ( 'NONE',  ( -1.529537955723671683, -64.35452850542924352, 5.030887037049979860 ) ) ;
#8235 = CARTESIAN_POINT ( 'NONE',  ( -4.725907263620355181, -62.59547149457074511, -1.635492904037597617 ) ) ;
#8236 = FILL_AREA_STYLE ('',( #3561 ) ) ;
#8237 = ORIENTED_EDGE ( 'NONE', *, *, #3976, .T. ) ;
#8238 = DIRECTION ( 'NONE',  ( 0.000000000000000000, 0.000000000000000000, -1.000000000000000000 ) ) ;
#8239 = EDGE_CURVE ( 'NONE', #4993, #8085, #3443, .T. ) ;
#8240 = VERTEX_POINT ( 'NONE', #4733 ) ;
#8241 = DIRECTION ( 'NONE',  ( 0.9954714945707483498, 0.09506052544079827971, -1.047588144072330487E-14 ) ) ;
#8242 = CARTESIAN_POINT ( 'NONE',  ( 5.257311121191341918, -74.25452850542924921, -0.09995255151729465215 ) ) ;
#8243 = CARTESIAN_POINT ( 'NONE',  ( -2.862020680886579349, -89.29547149457074795, -4.100960146803977580 ) ) ;
#8244 = CARTESIAN_POINT ( 'NONE',  ( -4.725907263620323207, -60.90452850542925489, 1.635492904037698647 ) ) ;
#8245 = CARTESIAN_POINT ( 'NONE',  ( 3.154386672714807549, -67.24547149457075079, 0.09995255151720662534 ) ) ;
#8246 = CARTESIAN_POINT ( 'NONE',  ( 2.179377348189481811, -77.85452850542925773, -7.030887037049986077 ) ) ;
#8247 = CARTESIAN_POINT ( 'NONE',  ( -5.257311121191322378, -92.74547149457073658, -0.09995255151718371311 ) ) ;
#8248 = CARTESIAN_POINT ( 'NONE',  ( -3.015831842038216415, -66.30452850542926058, -3.989209796945429432 ) ) ;
#8249 = CARTESIAN_POINT ( 'NONE',  ( 7.360235569667878508, -80.25452850542926342, -0.09995255151731691212 ) ) ;
#8250 = EDGE_CURVE ( 'NONE', #4876, #1902, #1499, .T. ) ;
#8251 = CARTESIAN_POINT ( 'NONE',  ( -1.840261337453199531, -84.19547149457073942, 2.371175808195584267 ) ) ;
#8252 = ORIENTED_EDGE ( 'NONE', *, *, #6810, .T. ) ;
#8253 = CARTESIAN_POINT ( 'NONE',  ( 50.00000000000000000, -9.999999999999992895, 4.499999999999999112 ) ) ;
#8254 = DIRECTION ( 'NONE',  ( 1.000000000000000000, 9.251858538542971581E-17, 0.000000000000000000 ) ) ;
#8255 = VERTEX_POINT ( 'NONE', #4150 ) ;
#8256 = CARTESIAN_POINT ( 'NONE',  ( -0.09506052544083846978, -90.00452850542924921, -4.999999999999997335 ) ) ;
#8257 = CARTESIAN_POINT ( 'NONE',  ( -2.823794231030023028, -60.90452850542925489, 1.017458915287783316 ) ) ;
#8258 = CARTESIAN_POINT ( 'NONE',  ( 4.191402346623195996, -61.80452850542926058, 5.607243785695311900 ) ) ;
#8259 = VECTOR ( 'NONE', #8254, 1000.000000000000000 ) ;
#8260 = VECTOR ( 'NONE', #1166, 1000.000000000000000 ) ;
#8261 = CARTESIAN_POINT ( 'NONE',  ( -7.360235569667858968, -68.74547149457075079, -0.09995255151716124498 ) ) ;
#8262 = CARTESIAN_POINT ( 'NONE',  ( 1.529537955723796028, -81.64547149457074227, 5.030887037049945221 ) ) ;
#8263 = CARTESIAN_POINT ( 'NONE',  ( 1.686450176301586001, -80.70452850542925205, -2.482926158054133303 ) ) ;
#8264 = VECTOR ( 'NONE', #7602, 1000.000000000000000 ) ;
#8265 = LINE ( 'NONE', #1826, #2954 ) ;
#8266 = ORIENTED_EDGE ( 'NONE', *, *, #7212, .T. ) ;
#8267 = CARTESIAN_POINT ( 'NONE',  ( -2.610703060766962569, -87.45452850542925205, -1.773238653441072232 ) ) ;
#8268 = CARTESIAN_POINT ( 'NONE',  ( -6.628020296210668683, -65.59547149457073090, -2.253526892787471869 ) ) ;
#8269 = LINE ( 'NONE', #7639, #4689 ) ;
#8270 = CARTESIAN_POINT ( 'NONE',  ( -4.784657899331159925, -65.89547149457074227, 1.454677039711874675 ) ) ;
#8271 = CARTESIAN_POINT ( 'NONE',  ( 4.191402346623081421, -94.69547149457076785, -5.607243785695398941 ) ) ;
#8272 = STYLED_ITEM ( 'NONE', ( #7318 ), #1832 ) ;
#8273 = CARTESIAN_POINT ( 'NONE',  ( -2.882544866740875289, -93.60452850542925773, -0.8366430509618996147 ) ) ;
#8274 = CARTESIAN_POINT ( 'NONE',  ( 6.000000000000006217, -51.00000000000000711, 2.500000000000000888 ) ) ;
#8275 = EDGE_CURVE ( 'NONE', #8040, #2655, #6006, .T. ) ;
#8276 = CARTESIAN_POINT ( 'NONE',  ( -4.784657899331191011, -69.60452850542925773, -1.454677039711773867 ) ) ;
#8277 = CARTESIAN_POINT ( 'NONE',  ( 0.09506052544075298261, -58.99547149457073658, -4.999999999999997335 ) ) ;
#8278 = ORIENTED_EDGE ( 'NONE', *, *, #8173, .T. ) ;
#8279 = LINE ( 'NONE', #2551, #2888 ) ;
#8280 = PRODUCT_CONTEXT ( 'NONE', #5766, 'mechanical' ) ;
#8281 = EDGE_LOOP ( 'NONE', ( #3539, #4930, #2355, #375 ) ) ;
#8282 = CARTESIAN_POINT ( 'NONE',  ( 1.500000000000002665, -27.00000000000000000, 4.500000000000000888 ) ) ;
#8283 = CARTESIAN_POINT ( 'NONE',  ( 4.784657899331210551, -80.10452850542925773, 1.454677039711774533 ) ) ;
#8284 = CARTESIAN_POINT ( 'NONE',  ( 1.719659006605286367, -85.84547149457075932, -4.969112962950050338 ) ) ;
#8285 = CARTESIAN_POINT ( 'NONE',  ( 4.069559105654484199, -96.99999999999998579, -1.141996675047574517 ) ) ;
#8286 = CARTESIAN_POINT ( 'NONE',  ( 2.493201789345309116, -69.94547149457073942, 1.934965279058241006 ) ) ;
#8287 = CARTESIAN_POINT ( 'NONE',  ( 6.013306294175169597, -82.95452850542925205, 4.245374608440616093 ) ) ;
#8288 = CARTESIAN_POINT ( 'NONE',  ( -2.862020680886579349, -86.29547149457074795, -4.100960146803977580 ) ) ;
#8289 = VECTOR ( 'NONE', #5189, 1000.000000000000000 ) ;
#8290 = CARTESIAN_POINT ( 'NONE',  ( 1.529537955723688336, -59.85452850542924352, -5.030887037049978971 ) ) ;
#8291 = CARTESIAN_POINT ( 'NONE',  ( -0.09506052544086139588, -75.00452850542926342, -6.999999999999997335 ) ) ;
#8292 = CARTESIAN_POINT ( 'NONE',  ( 2.493201789345311781, -90.94547149457073942, 1.934965279058241006 ) ) ;
#8293 = ORIENTED_EDGE ( 'NONE', *, *, #83, .F. ) ;
#8294 = CARTESIAN_POINT ( 'NONE',  ( -80.00000000000000000, 2.168404344971008868E-15, -12.50000000000000000 ) ) ;
#8295 = PLANE ( 'NONE',  #860 ) ;
#8296 = ORIENTED_EDGE ( 'NONE', *, *, #4829, .F. ) ;
#8297 = CARTESIAN_POINT ( 'NONE',  ( -1.719659006605370966, -87.15452850542926910, -4.969112962950015699 ) ) ;
#8298 = CARTESIAN_POINT ( 'NONE',  ( -1.069819614139472019, -96.34547149457074511, 2.969112962950044121 ) ) ;
#8299 = CARTESIAN_POINT ( 'NONE',  ( -4.191402346623181785, -57.30452850542924637, -5.607243785695311900 ) ) ;
#8300 = CARTESIAN_POINT ( 'NONE',  ( 2.369498399071075845, -67.84547149457071669, -6.969112962950057444 ) ) ;
#8301 = CARTESIAN_POINT ( 'NONE',  ( -4.725907263620352516, -86.59547149457075932, -1.635492904037597617 ) ) ;
#8302 = CARTESIAN_POINT ( 'NONE',  ( 2.493201789345272257, -80.55452850542926058, -1.934965279058294518 ) ) ;
#8303 = FACE_OUTER_BOUND ( 'NONE', #6091, .T. ) ;
#8304 = CARTESIAN_POINT ( 'NONE',  ( 2.882544866740897493, -86.10452850542924352, 0.8366430509618999478 ) ) ;
#8305 = CARTESIAN_POINT ( 'NONE',  ( 7.360235569667880284, -95.25452850542926342, -0.09995255151731691212 ) ) ;
#8306 = ADVANCED_FACE ( 'NONE', ( #6721 ), #952, .T. ) ;
#8307 =( REPRESENTATION_RELATIONSHIP ('NONE','NONE', #4188, #1989 ) REPRESENTATION_RELATIONSHIP_WITH_TRANSFORMATION ( #59 )SHAPE_REPRESENTATION_RELATIONSHIP( ) );
#8308 = CARTESIAN_POINT ( 'NONE',  ( 75.00000000000000000, -20.00000000000000000, -7.500000000000000000 ) ) ;
#8309 = PRODUCT_DEFINITION_SHAPE ( 'NONE', 'NONE',  #1135 ) ;
#8310 = CARTESIAN_POINT ( 'NONE',  ( 3.015831842038147581, -67.69547149457073942, -3.989209796945492048 ) ) ;
#8311 = CARTESIAN_POINT ( 'NONE',  ( -1.719659006605267493, -63.34547149457075221, 4.969112962950051227 ) ) ;
#8312 = CARTESIAN_POINT ( 'NONE',  ( 2.610703060766986106, -91.95452850542925205, 1.773238653441072232 ) ) ;
#8313 = ADVANCED_FACE ( 'NONE', ( #7273 ), #4066, .F. ) ;
#8314 = FACE_OUTER_BOUND ( 'NONE', #1367, .T. ) ;
#8315 = AXIS2_PLACEMENT_3D ( 'NONE', #4894, #2994, #8181 ) ;
#8316 = CARTESIAN_POINT ( 'NONE',  ( -4.312004677471058756, -69.45452850542925205, -3.009306630940844052 ) ) ;
#8317 = CARTESIAN_POINT ( 'NONE',  ( -0.09506052544071229293, -90.49547149457075079, 6.999999999999997335 ) ) ;
#8318 =( NAMED_UNIT ( * ) PLANE_ANGLE_UNIT ( ) SI_UNIT ( $, .RADIAN. ) );
#8319 = ORIENTED_EDGE ( 'NONE', *, *, #2667, .F. ) ;
#8320 = CARTESIAN_POINT ( 'NONE',  ( 6.123233995736760366E-16, -26.99999999999998934, -7.000000000000000000 ) ) ;
#8321 = ITEM_DEFINED_TRANSFORMATION ( 'NONE', 'NONE', #5502,  #2840 ) ;
#8322 = VERTEX_POINT ( 'NONE', #908 ) ;
#8323 = DIRECTION ( 'NONE',  ( 0.000000000000000000, 0.000000000000000000, -1.000000000000000000 ) ) ;
#8324 = CARTESIAN_POINT ( 'NONE',  ( 3.015831842038233734, -76.80452850542926058, 3.989209796945429432 ) ) ;
#8325 = CARTESIAN_POINT ( 'NONE',  ( 0.09506052544075600796, -82.99547149457075079, -4.999999999999997335 ) ) ;
#8326 = CARTESIAN_POINT ( 'NONE',  ( 3.305848925379873293, -97.00000000000001421, -2.438564738088757622 ) ) ;
#8327 = CARTESIAN_POINT ( 'NONE',  ( 2.882544866740876621, -70.39547149457072805, -0.8366430509619593447 ) ) ;
#8328 = AXIS2_PLACEMENT_3D ( 'NONE', #3159, #3328, #116 ) ;
#8329 = CARTESIAN_POINT ( 'NONE',  ( 4.191402346623198660, -82.80452850542926058, 5.607243785695311900 ) ) ;
#8330 = CARTESIAN_POINT ( 'NONE',  ( -5.257311121191324155, -77.74547149457070816, -0.09995255151718371311 ) ) ;
#8331 = CARTESIAN_POINT ( 'NONE',  ( -4.194503406049321370, -58.05452850542925347, 3.171033256558100533 ) ) ;
#8332 = CARTESIAN_POINT ( 'NONE',  ( -3.015831842038213306, -93.30452850542926058, -3.989209796945429432 ) ) ;
#8333 = CARTESIAN_POINT ( 'NONE',  ( 4.191402346623198660, -79.80452850542926058, 5.607243785695311900 ) ) ;
#8334 = CARTESIAN_POINT ( 'NONE',  ( -2.882544866740857081, -83.89547149457074227, 0.8366430509619596778 ) ) ;
#8335 = EDGE_CURVE ( 'NONE', #1092, #3690, #5414, .T. ) ;
#8336 = ORIENTED_EDGE ( 'NONE', *, *, #6646, .F. ) ;
#8337 = CARTESIAN_POINT ( 'NONE',  ( -3.154386672714788453, -84.75452850542926342, 0.09995255151727280851 ) ) ;
#8338 = NEXT_ASSEMBLY_USAGE_OCCURRENCE ( 'NAUO1', ' ', ' ', #1497, #3506, $ ) ;
#8339 = NEXT_ASSEMBLY_USAGE_OCCURRENCE ( 'NAUO2', ' ', ' ', #1497, #1135, $ ) ;
#8340 = NEXT_ASSEMBLY_USAGE_OCCURRENCE ( 'NAUO3', ' ', ' ', #1497, #2017, $ ) ;
#8341 = NEXT_ASSEMBLY_USAGE_OCCURRENCE ( 'NAUO4', ' ', ' ', #1497, #5608, $ ) ;
#8342 = NEXT_ASSEMBLY_USAGE_OCCURRENCE ( 'NAUO5', ' ', ' ', #1497, #1392, $ ) ;
#8343 = NEXT_ASSEMBLY_USAGE_OCCURRENCE ( 'NAUO6', ' ', ' ', #1497, #5865, $ ) ;
#8344 = NEXT_ASSEMBLY_USAGE_OCCURRENCE ( 'NAUO7', ' ', ' ', #1497, #1135, $ ) ;
#8345 = NEXT_ASSEMBLY_USAGE_OCCURRENCE ( 'NAUO8', ' ', ' ', #1497, #2017, $ ) ;
#8346 = NEXT_ASSEMBLY_USAGE_OCCURRENCE ( 'NAUO9', ' ', ' ', #1497, #1392, $ ) ;
#8347 = NEXT_ASSEMBLY_USAGE_OCCURRENCE ( 'NAUO10', ' ', ' ', #1497, #5357, $ ) ;
#8348 = NEXT_ASSEMBLY_USAGE_OCCURRENCE ( 'NAUO11', ' ', ' ', #1497, #5357, $ ) ;
#8349 = NEXT_ASSEMBLY_USAGE_OCCURRENCE ( 'NAUO12', ' ', ' ', #1497, #6847, $ ) ;
#8350 = NEXT_ASSEMBLY_USAGE_OCCURRENCE ( 'NAUO13', ' ', ' ', #1497, #6847, $ ) ;
ENDSEC;
END-ISO-10303-21;
